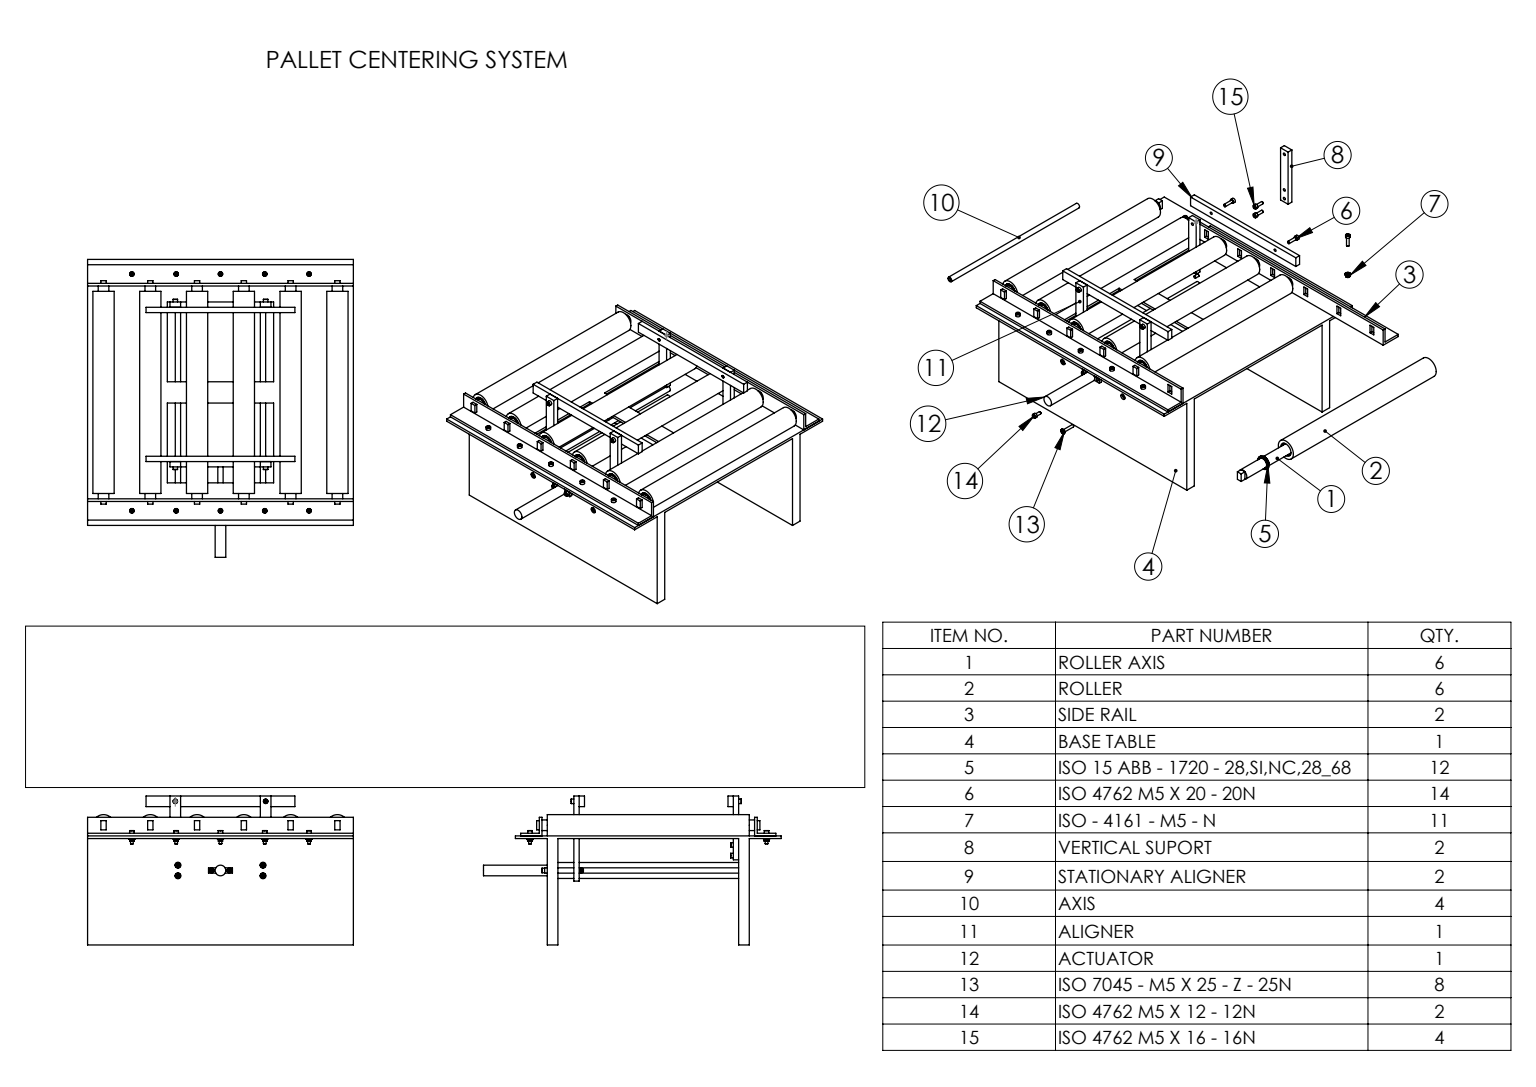
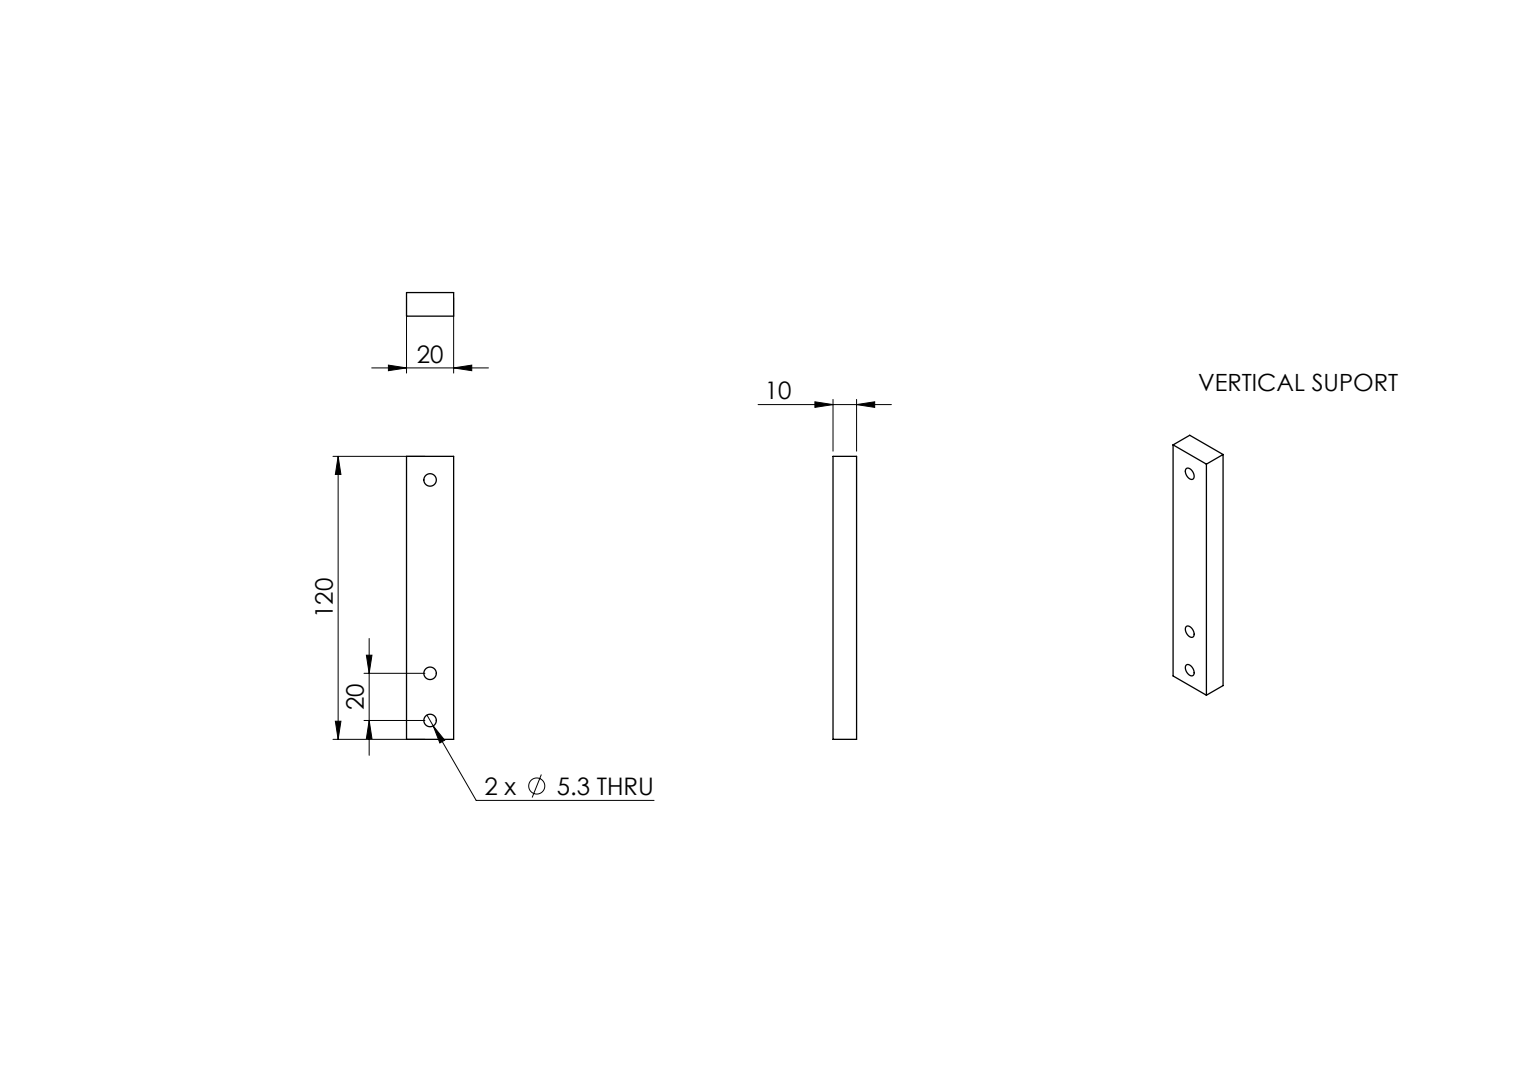
ISO-10303-21;
HEADER;
FILE_DESCRIPTION (('STEP AP214'),
    '1' );
FILE_NAME ('MAS-197',
    '2026-10-24T13:33:06',
    ( '' ),
    ( '' ),
    'SwSTEP 2.0',
    'SolidWorks 2026',
    '' );
FILE_SCHEMA (( 'AUTOMOTIVE_DESIGN' ));
ENDSEC;

DATA;
#1 = CARTESIAN_POINT ( 'NONE',  ( 53.33333333333330017, -25.00000000000000000, 222.5000000000000853 ) ) ;
#2 = AXIS2_PLACEMENT_3D ( 'NONE', #1029, #14245, #1184 ) ;
#3 = ORIENTED_EDGE ( 'NONE', *, *, #4024, .T. ) ;
#4 = CARTESIAN_POINT ( 'NONE',  ( 302.6499999999999204, -75.00000000000008527, 169.9999999999999716 ) ) ;
#5 = CARTESIAN_POINT ( 'NONE',  ( 136.6666666666666288, -20.00000000000000000, -219.8500000000001080 ) ) ;
#6 = DIRECTION ( 'NONE',  ( 0.000000000000000000, 0.000000000000000000, -1.000000000000000000 ) ) ;
#7 = EDGE_LOOP ( 'NONE', ( #4823, #10214, #8474, #13193, #10057 ) ) ;
#8 = COLOUR_RGB ( '',0.8941176470588234615, 0.8941176470588234615, 0.8941176470588234615 ) ;
#9 = EDGE_CURVE ( 'NONE', #9071, #5710, #2897, .T. ) ;
#10 = DIRECTION ( 'NONE',  ( 0.000000000000000000, 0.000000000000000000, -1.000000000000000000 ) ) ;
#11 = EDGE_CURVE ( 'NONE', #2602, #678, #10776, .T. ) ;
#12 = LINE ( 'NONE', #10262, #8342 ) ;
#13 = LINE ( 'NONE', #14246, #12970 ) ;
#14 = AXIS2_PLACEMENT_3D ( 'NONE', #7611, #4365, #10700 ) ;
#15 = DIRECTION ( 'NONE',  ( -0.000000000000000000, -0.000000000000000000, -1.000000000000000000 ) ) ;
#16 = EDGE_CURVE ( 'NONE', #12113, #10379, #13864, .T. ) ;
#17 = ORIENTED_EDGE ( 'NONE', *, *, #13765, .F. ) ;
#18 = MECHANICAL_DESIGN_GEOMETRIC_PRESENTATION_REPRESENTATION (  '', ( #6765 ), #7674 ) ;
#19 = DIRECTION ( 'NONE',  ( 1.000000000000000000, 0.000000000000000000, 0.000000000000000000 ) ) ;
#20 = DIRECTION ( 'NONE',  ( 1.000000000000000000, 0.000000000000000000, 0.000000000000000000 ) ) ;
#21 = VECTOR ( 'NONE', #6060, 1000.000000000000000 ) ;
#22 = CARTESIAN_POINT ( 'NONE',  ( 137.4999999999999432, -36.99999999999997868, -180.0000000000000000 ) ) ;
#23 = ORIENTED_EDGE ( 'NONE', *, *, #5278, .F. ) ;
#24 = CYLINDRICAL_SURFACE ( 'NONE', #7328, 2.649999999999985700 ) ;
#25 = AXIS2_PLACEMENT_3D ( 'NONE', #8308, #3030, #675 ) ;
#26 = COLOUR_RGB ( '',0.8941176470588234615, 0.8941176470588234615, 0.8941176470588234615 ) ;
#27 = DIRECTION ( 'NONE',  ( -0.000000000000000000, 0.000000000000000000, -1.000000000000000000 ) ) ;
#28 = VECTOR ( 'NONE', #11250, 999.9999999999997726 ) ;
#29 = CARTESIAN_POINT ( 'NONE',  ( 302.6499999999999204, -75.00000000000008527, 186.2999999999999829 ) ) ;
#30 = DIRECTION ( 'NONE',  ( 1.000000000000000000, 6.123233995736766036E-17, -6.123233995736764803E-17 ) ) ;
#31 = AXIS2_PLACEMENT_3D ( 'NONE', #13162, #68, #13234 ) ;
#32 = VERTEX_POINT ( 'NONE', #10617 ) ;
#33 = DIRECTION ( 'NONE',  ( -1.000000000000000000, -0.000000000000000000, -0.000000000000000000 ) ) ;
#34 = EDGE_CURVE ( 'NONE', #3584, #3648, #12190, .T. ) ;
#35 =( GEOMETRIC_REPRESENTATION_CONTEXT ( 3 ) GLOBAL_UNCERTAINTY_ASSIGNED_CONTEXT ( ( #12045 ) ) GLOBAL_UNIT_ASSIGNED_CONTEXT ( ( #1891, #1958, #13996 ) ) REPRESENTATION_CONTEXT ( 'NONE', 'WORKASPACE' ) );
#36 = ORIENTED_EDGE ( 'NONE', *, *, #2375, .F. ) ;
#37 = ADVANCED_FACE ( 'NONE', ( #11695 ), #12926, .T. ) ;
#38 = CARTESIAN_POINT ( 'NONE',  ( 4.175648173966055587, -2.207990556236547608, -3.469390959564065291 ) ) ;
#39 = ORIENTED_EDGE ( 'NONE', *, *, #7804, .T. ) ;
#40 = ORIENTED_EDGE ( 'NONE', *, *, #13656, .T. ) ;
#41 = CARTESIAN_POINT ( 'NONE',  ( 2.000000000000001332, 13.29999999999999893, 0.000000000000000000 ) ) ;
#42 = FACE_OUTER_BOUND ( 'NONE', #11021, .T. ) ;
#43 = CIRCLE ( 'NONE', #4245, 0.2000000000000000944 ) ;
#44 = DIRECTION ( 'NONE',  ( -0.000000000000000000, -0.000000000000000000, 1.000000000000000000 ) ) ;
#45 = CARTESIAN_POINT ( 'NONE',  ( 386.6666666666666288, -20.00000000000000000, 225.1500000000000625 ) ) ;
#46 = FACE_OUTER_BOUND ( 'NONE', #11584, .T. ) ;
#47 = CARTESIAN_POINT ( 'NONE',  ( -30.00000000000002842, -25.00000000000000000, 250.0000000000000000 ) ) ;
#48 = PLANE ( 'NONE',  #10641 ) ;
#49 = DIRECTION ( 'NONE',  ( 1.000000000000000000, 0.000000000000000000, 0.000000000000000000 ) ) ;
#50 = VERTEX_POINT ( 'NONE', #7335 ) ;
#51 = ORIENTED_EDGE ( 'NONE', *, *, #14217, .F. ) ;
#52 = FACE_OUTER_BOUND ( 'NONE', #5422, .T. ) ;
#53 = ORIENTED_EDGE ( 'NONE', *, *, #841, .T. ) ;
#54 = CARTESIAN_POINT ( 'NONE',  ( -299.9999999999999432, -75.00000000000008527, 329.9999999999999432 ) ) ;
#55 = ORIENTED_EDGE ( 'NONE', *, *, #9775, .T. ) ;
#56 = DIRECTION ( 'NONE',  ( 1.000000000000000000, 0.000000000000000000, 0.000000000000000000 ) ) ;
#57 = ORIENTED_EDGE ( 'NONE', *, *, #5179, .T. ) ;
#58 = CARTESIAN_POINT ( 'NONE',  ( -297.4999999999999432, -75.00000000000008527, 10.00000000000000178 ) ) ;
#59 = PRODUCT ( 'MAS-197', 'MAS-197', '', ( #13427 ) ) ;
#60 = CARTESIAN_POINT ( 'NONE',  ( 4.000000000000000000, 2.309401076758497151, -3.433295621305379353 ) ) ;
#61 = DIRECTION ( 'NONE',  ( -1.000000000000000000, -0.000000000000000000, -0.000000000000000000 ) ) ;
#62 = EDGE_CURVE ( 'NONE', #11600, #2281, #14003, .T. ) ;
#63 = CARTESIAN_POINT ( 'NONE',  ( 2.500000000000000000, 0.000000000000000000, 0.000000000000000000 ) ) ;
#64 = EDGE_CURVE ( 'NONE', #764, #13509, #648, .T. ) ;
#65 = CARTESIAN_POINT ( 'NONE',  ( -30.00000000000002842, -20.00000000000000000, 250.0000000000000000 ) ) ;
#66 = ORIENTED_EDGE ( 'NONE', *, *, #8156, .T. ) ;
#67 = VERTEX_POINT ( 'NONE', #13720 ) ;
#68 = DIRECTION ( 'NONE',  ( 1.000000000000000000, 0.000000000000000000, 0.000000000000000000 ) ) ;
#69 = ORIENTED_EDGE ( 'NONE', *, *, #9344, .T. ) ;
#70 = DIRECTION ( 'NONE',  ( 0.000000000000000000, 1.000000000000000000, 0.000000000000000000 ) ) ;
#71 = CYLINDRICAL_SURFACE ( 'NONE', #9896, 2.500000000000000444 ) ;
#72 =( NAMED_UNIT ( * ) SI_UNIT ( $, .STERADIAN. ) SOLID_ANGLE_UNIT ( ) );
#73 =( REPRESENTATION_RELATIONSHIP ('NONE','NONE', #11251, #2275 ) REPRESENTATION_RELATIONSHIP_WITH_TRANSFORMATION ( #10001 )SHAPE_REPRESENTATION_RELATIONSHIP( ) );
#74 = EDGE_CURVE ( 'NONE', #2665, #8392, #9526, .T. ) ;
#75 = PRODUCT_DEFINITION ( 'UNKNOWN', '', #10251, #12968 ) ;
#76 = LINE ( 'NONE', #7062, #6983 ) ;
#77 = FACE_OUTER_BOUND ( 'NONE', #3479, .T. ) ;
#78 = PLANE ( 'NONE',  #3254 ) ;
#79 = DIRECTION ( 'NONE',  ( 1.000000000000000000, 0.000000000000000000, 0.000000000000000000 ) ) ;
#80 = EDGE_LOOP ( 'NONE', ( #13793, #10829, #6578 ) ) ;
#81 = ADVANCED_FACE ( 'NONE', ( #7413, #11845, #1899, #419, #4888, #9306, #3544 ), #4372, .T. ) ;
#82 = EDGE_CURVE ( 'NONE', #232, #4077, #12381, .T. ) ;
#83 = AXIS2_PLACEMENT_3D ( 'NONE', #9067, #7962, #321 ) ;
#84 = AXIS2_PLACEMENT_3D ( 'NONE', #4836, #3666, #8077 ) ;
#85 = EDGE_CURVE ( 'NONE', #6756, #11518, #12060, .T. ) ;
#86 = ADVANCED_FACE ( 'NONE', ( #14292 ), #14148, .F. ) ;
#87 = CARTESIAN_POINT ( 'NONE',  ( 134.9999999999999432, -36.99999999999997868, 0.000000000000000000 ) ) ;
#88 = LINE ( 'NONE', #2296, #2370 ) ;
#89 = PLANE ( 'NONE',  #11765 ) ;
#90 = ORIENTED_EDGE ( 'NONE', *, *, #8678, .T. ) ;
#91 = ADVANCED_FACE ( 'NONE', ( #1003 ), #2259, .T. ) ;
#92 = CARTESIAN_POINT ( 'NONE',  ( -144.9999999999999432, -105.0000000000000853, 40.00000000000000000 ) ) ;
#93 = CARTESIAN_POINT ( 'NONE',  ( 2.500000000000000000, 2.357898499370433054, -1.951563910473907981E-15 ) ) ;
#94 = DIRECTION ( 'NONE',  ( 0.000000000000000000, 0.000000000000000000, 1.000000000000000000 ) ) ;
#95 = CIRCLE ( 'NONE', #11951, 2.700000000000000178 ) ;
#96 = ORIENTED_EDGE ( 'NONE', *, *, #5946, .F. ) ;
#97 = LINE ( 'NONE', #13393, #5781 ) ;
#98 = ORIENTED_EDGE ( 'NONE', *, *, #4977, .T. ) ;
#99 = CARTESIAN_POINT ( 'NONE',  ( 4.999999999999997335, 0.000000000000000000, 4.250000000000000000 ) ) ;
#100 = VECTOR ( 'NONE', #4876, 1000.000000000000000 ) ;
#101 = ORIENTED_EDGE ( 'NONE', *, *, #7387, .T. ) ;
#102 = ORIENTED_EDGE ( 'NONE', *, *, #13999, .T. ) ;
#103 = DIRECTION ( 'NONE',  ( -1.000000000000000000, 0.000000000000000000, 0.000000000000000000 ) ) ;
#104 = DIRECTION ( 'NONE',  ( 0.000000000000000000, 0.000000000000000000, 1.000000000000000000 ) ) ;
#105 = CARTESIAN_POINT ( 'NONE',  ( 5.000000000000000888, 0.000000000000000000, 0.000000000000000000 ) ) ;
#106 = DIRECTION ( 'NONE',  ( 0.4461977533473793778, 0.8949343913984707521, -1.884057886186824495E-16 ) ) ;
#107 = LINE ( 'NONE', #12182, #1892 ) ;
#108 = LINE ( 'NONE', #6679, #5937 ) ;
#109 = SURFACE_STYLE_FILL_AREA ( #5656 ) ;
#110 = EDGE_CURVE ( 'NONE', #13194, #10462, #10760, .T. ) ;
#111 = CARTESIAN_POINT ( 'NONE',  ( 132.4999999999999432, -36.99999999999997868, -169.9999999999999716 ) ) ;
#112 = ITEM_DEFINED_TRANSFORMATION ( 'NONE', 'NONE', #8858,  #14039 ) ;
#113 = CIRCLE ( 'NONE', #1517, 5.500000000000005329 ) ;
#114 = ORIENTED_EDGE ( 'NONE', *, *, #1574, .F. ) ;
#115 = ORIENTED_EDGE ( 'NONE', *, *, #82, .F. ) ;
#116 = AXIS2_PLACEMENT_3D ( 'NONE', #1990, #12809, #3959 ) ;
#117 = CARTESIAN_POINT ( 'NONE',  ( 0.06760930072668894231, 0.9010842325122832008, -0.5150000000000000133 ) ) ;
#118 = ORIENTED_EDGE ( 'NONE', *, *, #14031, .F. ) ;
#119 = CARTESIAN_POINT ( 'NONE',  ( 134.5000000000000000, -95.00000000000008527, 190.0000000000000000 ) ) ;
#120 = AXIS2_PLACEMENT_3D ( 'NONE', #1147, #9264, #49 ) ;
#121 = ORIENTED_EDGE ( 'NONE', *, *, #4725, .F. ) ;
#122 = LINE ( 'NONE', #2191, #4564 ) ;
#123 = ORIENTED_EDGE ( 'NONE', *, *, #13765, .T. ) ;
#124 = CARTESIAN_POINT ( 'NONE',  ( 142.6500000000000057, -95.00000000000008527, 190.0000000000000000 ) ) ;
#125 = AXIS2_PLACEMENT_3D ( 'NONE', #612, #5076, #9487 ) ;
#126 = CARTESIAN_POINT ( 'NONE',  ( 4.000000000000000888, 1.539600717838996990, -3.300726591567079815 ) ) ;
#127 = DIRECTION ( 'NONE',  ( 0.000000000000000000, 0.000000000000000000, 1.000000000000000000 ) ) ;
#128 = AXIS2_PLACEMENT_3D ( 'NONE', #6258, #5252, #1681 ) ;
#129 = CARTESIAN_POINT ( 'NONE',  ( 357.0000000000000000, 8.660254037844390851, 205.0000000000000284 ) ) ;
#130 = FILL_AREA_STYLE ('',( #3509 ) ) ;
#131 = DIRECTION ( 'NONE',  ( 0.4461977533474923430, -0.8949343913984144638, 0.000000000000000000 ) ) ;
#132 = DIRECTION ( 'NONE',  ( 1.000000000000000000, 0.000000000000000000, 0.000000000000000000 ) ) ;
#133 = DIRECTION ( 'NONE',  ( 1.000000000000000000, 0.000000000000000000, 0.000000000000000000 ) ) ;
#134 = VECTOR ( 'NONE', #9384, 1000.000000000000000 ) ;
#135 =( REPRESENTATION_RELATIONSHIP ('NONE','NONE', #11251, #5332 ) REPRESENTATION_RELATIONSHIP_WITH_TRANSFORMATION ( #4005 )SHAPE_REPRESENTATION_RELATIONSHIP( ) );
#136 = EDGE_LOOP ( 'NONE', ( #496, #11440, #13448, #1824 ) ) ;
#137 = ORIENTED_EDGE ( 'NONE', *, *, #8244, .F. ) ;
#138 = VECTOR ( 'NONE', #5329, 1000.000000000000000 ) ;
#139 = B_SPLINE_CURVE_WITH_KNOTS ( 'NONE', 3,
 ( #12728, #3886, #6926, #516, #12587, #8082 ),
 .UNSPECIFIED., .F., .F.,
 ( 4, 2, 4 ),
 ( 0.002365888236227967761, 0.003551327329835077609, 0.004736766423442186590 ),
 .UNSPECIFIED. ) ;
#140 = VERTEX_POINT ( 'NONE', #5318 ) ;
#141 = ADVANCED_FACE ( 'NONE', ( #13281 ), #9741, .F. ) ;
#143 = CARTESIAN_POINT ( 'NONE',  ( 93.00000000000000000, -8.660254037844389075, 199.9990000000000236 ) ) ;
#142 = AXIS2_PLACEMENT_3D ( 'NONE', #8631, #1337, #6858 ) ;
#144 = VECTOR ( 'NONE', #12485, 1000.000000000000000 ) ;
#145 = VERTEX_POINT ( 'NONE', #3075 ) ;
#146 = CARTESIAN_POINT ( 'NONE',  ( 0.000000000000000000, -2.349999999999999201, 0.5149999999999992362 ) ) ;
#147 = DIRECTION ( 'NONE',  ( 0.000000000000000000, 0.000000000000000000, 1.000000000000000000 ) ) ;
#148 = CIRCLE ( 'NONE', #8278, 4.000000000000000000 ) ;
#149 = AXIS2_PLACEMENT_3D ( 'NONE', #12993, #2990, #1889 ) ;
#150 = LINE ( 'NONE', #1253, #5148 ) ;
#151 = FACE_OUTER_BOUND ( 'NONE', #9117, .T. ) ;
#152 = AXIS2_PLACEMENT_3D ( 'NONE', #10051, #218, #9907 ) ;
#153 = PLANE ( 'NONE',  #6564 ) ;
#154 = DIRECTION ( 'NONE',  ( 1.000000000000000000, 0.000000000000000000, 0.000000000000000000 ) ) ;
#155 = EDGE_LOOP ( 'NONE', ( #7067, #11901, #14288, #9379, #2172, #12925 ) ) ;
#156 = ADVANCED_FACE ( 'NONE', ( #2113 ), #8789, .F. ) ;
#157 = DIRECTION ( 'NONE',  ( -0.000000000000000000, -0.000000000000000000, 1.000000000000000000 ) ) ;
#158 = CYLINDRICAL_SURFACE ( 'NONE', #4474, 2.649999999999985700 ) ;
#159=STYLED_ITEM('',(#14424),#13163);
#160 = CARTESIAN_POINT ( 'NONE',  ( 2.500000000000000000, -1.178949249685218303, -2.041999999999998039 ) ) ;
#161 = VERTEX_POINT ( 'NONE', #11045 ) ;
#162 = DIRECTION ( 'NONE',  ( -0.000000000000000000, -0.000000000000000000, 1.000000000000000000 ) ) ;
#163 = ADVANCED_FACE ( 'NONE', ( #5247 ), #3288, .T. ) ;
#164 = EDGE_CURVE ( 'NONE', #13531, #14219, #11463, .T. ) ;
#165 = CARTESIAN_POINT ( 'NONE',  ( 5.000000000000000888, 4.250000000000000000, 0.000000000000000000 ) ) ;
#166 = DIRECTION ( 'NONE',  ( 1.000000000000000000, 0.000000000000000000, 0.000000000000000000 ) ) ;
#167 = EDGE_CURVE ( 'NONE', #11965, #7113, #13067, .T. ) ;
#168 = VECTOR ( 'NONE', #12487, 1000.000000000000000 ) ;
#169 = ITEM_DEFINED_TRANSFORMATION ( 'NONE', 'NONE', #949,  #14039 ) ;
#170 = ORIENTED_EDGE ( 'NONE', *, *, #8134, .F. ) ;
#171 = CIRCLE ( 'NONE', #3238, 20.00000000000000000 ) ;
#172 = CARTESIAN_POINT ( 'NONE',  ( 21.00000000000000355, 0.000000000000000000, 0.000000000000000000 ) ) ;
#173 = PRODUCT ( 'base table', 'base table', '', ( #338 ) ) ;
#174 = B_SPLINE_CURVE_WITH_KNOTS ( 'NONE', 3,
 ( #13860, #2775, #7121, #12779, #11548 ),
 .UNSPECIFIED., .F., .F.,
 ( 4, 1, 4 ),
 ( 0.000000000000000000, 0.002309401076758506657, 0.004618802153517013315 ),
 .UNSPECIFIED. ) ;
#175 = ORIENTED_EDGE ( 'NONE', *, *, #6775, .T. ) ;
#176 = DIRECTION ( 'NONE',  ( -0.000000000000000000, 1.000000000000000000, 0.000000000000000000 ) ) ;
#177 = CIRCLE ( 'NONE', #2061, 2.500000000000002220 ) ;
#178 = ORIENTED_EDGE ( 'NONE', *, *, #7566, .F. ) ;
#179 = ORIENTED_EDGE ( 'NONE', *, *, #5778, .F. ) ;
#180 = CARTESIAN_POINT ( 'NONE',  ( 299.9999999999999432, -95.00000000000008527, 190.0000000000000000 ) ) ;
#181 = CARTESIAN_POINT ( 'NONE',  ( 302.6499999999999204, -95.00000000000008527, -186.2999999999999829 ) ) ;
#182 = CARTESIAN_POINT ( 'NONE',  ( 2.500000000000000000, -1.768423874527823791, -1.020999999999998353 ) ) ;
#183 = VECTOR ( 'NONE', #12816, 1000.000000000000000 ) ;
#184 = FACE_OUTER_BOUND ( 'NONE', #8422, .T. ) ;
#185 = DIRECTION ( 'NONE',  ( 1.000000000000000000, 0.000000000000000000, 0.000000000000000000 ) ) ;
#186 = DIRECTION ( 'NONE',  ( 1.000000000000000000, 0.000000000000000000, 0.000000000000000000 ) ) ;
#187 =( LENGTH_UNIT ( ) NAMED_UNIT ( * ) SI_UNIT ( .MILLI., .METRE. ) );
#188 = EDGE_CURVE ( 'NONE', #1051, #13344, #1074, .T. ) ;
#189 = CARTESIAN_POINT ( 'NONE',  ( 4.207491450040567571, -2.029819825146485179, -3.671670828759567407 ) ) ;
#190 = EDGE_LOOP ( 'NONE', ( #1618, #1963 ) ) ;
#191 = VERTEX_POINT ( 'NONE', #7546 ) ;
#192 = CARTESIAN_POINT ( 'NONE',  ( 303.3333333333333144, -20.00000000000000000, -219.8500000000001080 ) ) ;
#193 = ORIENTED_EDGE ( 'NONE', *, *, #7276, .F. ) ;
#194 = DIRECTION ( 'NONE',  ( 1.000000000000000000, 0.000000000000000000, 0.000000000000000000 ) ) ;
#195 = CIRCLE ( 'NONE', #13619, 2.500000000000002220 ) ;
#196 = EDGE_LOOP ( 'NONE', ( #178, #7479, #11699, #10408 ) ) ;
#197 = DIRECTION ( 'NONE',  ( -0.000000000000000000, -0.000000000000000000, -1.000000000000000000 ) ) ;
#198 = ORIENTED_EDGE ( 'NONE', *, *, #12237, .T. ) ;
#199 = AXIS2_PLACEMENT_3D ( 'NONE', #13030, #8676, #7512 ) ;
#200 = CARTESIAN_POINT ( 'NONE',  ( -294.9999999999999432, -75.00000000000008527, 339.9999999999999432 ) ) ;
#201 = CARTESIAN_POINT ( 'NONE',  ( 294.4999999999999432, -75.00000000000008527, -190.0000000000000000 ) ) ;
#202 = DIRECTION ( 'NONE',  ( -0.000000000000000000, 0.000000000000000000, -1.000000000000000000 ) ) ;
#203 = DIRECTION ( 'NONE',  ( 0.000000000000000000, 0.000000000000000000, 1.000000000000000000 ) ) ;
#204 = PRESENTATION_STYLE_ASSIGNMENT (( #4594 ) ) ;
#205 = CYLINDRICAL_SURFACE ( 'NONE', #8810, 11.05000000000000071 ) ;
#206 = SHAPE_DEFINITION_REPRESENTATION ( #7042, #11251 ) ;
#207 = DIRECTION ( 'NONE',  ( 0.000000000000000000, -0.000000000000000000, 1.000000000000000000 ) ) ;
#208 = SHAPE_REPRESENTATION ( 'angular contact ball bearing_68_iso_ISO 15 ABB - 1720 - 28,SI,NC,28_68', ( #14039 ), #11646 ) ;
#209 = ORIENTED_EDGE ( 'NONE', *, *, #9578, .T. ) ;
#210 = ORIENTED_EDGE ( 'NONE', *, *, #2503, .T. ) ;
#211 = ORIENTED_EDGE ( 'NONE', *, *, #1146, .F. ) ;
#212 = VECTOR ( 'NONE', #10286, 1000.000000000000114 ) ;
#213 = CARTESIAN_POINT ( 'NONE',  ( 3.383466608491643077E-15, 4.736522675502341073, -3.681124513963742739 ) ) ;
#214 = EDGE_CURVE ( 'NONE', #1600, #9602, #14242, .T. ) ;
#215 = ORIENTED_EDGE ( 'NONE', *, *, #12757, .F. ) ;
#216 = CYLINDRICAL_SURFACE ( 'NONE', #14049, 4.250000000000000000 ) ;
#217 = PLANE ( 'NONE',  #14054 ) ;
#218 = DIRECTION ( 'NONE',  ( -1.000000000000000000, -0.000000000000000000, -0.000000000000000000 ) ) ;
#219 = CIRCLE ( 'NONE', #5381, 5.000000000000004441 ) ;
#220 = AXIS2_PLACEMENT_3D ( 'NONE', #2707, #9091, #281 ) ;
#221 = CARTESIAN_POINT ( 'NONE',  ( -25.39999999999996305, 0.000000000000000000, 0.000000000000000000 ) ) ;
#222 = VECTOR ( 'NONE', #1616, 1000.000000000000000 ) ;
#223 = LINE ( 'NONE', #12223, #5365 ) ;
#224 = CARTESIAN_POINT ( 'NONE',  ( -219.9999999999999147, -85.00000000000009948, 30.00000000000000000 ) ) ;
#225 = CARTESIAN_POINT ( 'NONE',  ( 8.000000000000000000, -4.837354856632045452E-15, -0.5150000000000000133 ) ) ;
#226 = EDGE_LOOP ( 'NONE', ( #6646, #8713, #11419, #2781 ) ) ;
#227 = FILL_AREA_STYLE ('',( #2582 ) ) ;
#228 = AXIS2_PLACEMENT_3D ( 'NONE', #3013, #14095, #2869 ) ;
#229 = DIRECTION ( 'NONE',  ( -0.000000000000000000, -0.000000000000000000, -1.000000000000000000 ) ) ;
#230 = LINE ( 'NONE', #296, #13478 ) ;
#231 = LINE ( 'NONE', #7733, #9690 ) ;
#232 = VERTEX_POINT ( 'NONE', #2038 ) ;
#233 = FACE_OUTER_BOUND ( 'NONE', #9286, .T. ) ;
#234 = EDGE_CURVE ( 'NONE', #10453, #9107, #4526, .T. ) ;
#235 = AXIS2_PLACEMENT_3D ( 'NONE', #10662, #12975, #4053 ) ;
#236 = DIRECTION ( 'NONE',  ( 1.000000000000000000, 0.000000000000000000, 0.000000000000000000 ) ) ;
#237 = DIRECTION ( 'NONE',  ( 0.000000000000000000, 0.000000000000000000, 1.000000000000000000 ) ) ;
#238 = EDGE_CURVE ( 'NONE', #5881, #9436, #12617, .T. ) ;
#239 = ORIENTED_EDGE ( 'NONE', *, *, #12866, .T. ) ;
#240 = DIRECTION ( 'NONE',  ( 0.000000000000000000, 1.000000000000000000, -1.224646799147353207E-16 ) ) ;
#241 = AXIS2_PLACEMENT_3D ( 'NONE', #10628, #13202, #658 ) ;
#242 = ORIENTED_EDGE ( 'NONE', *, *, #12141, .F. ) ;
#243 = CARTESIAN_POINT ( 'NONE',  ( 4.141042297810615835, -2.227970268150433863, -3.687027686973623819 ) ) ;
#244 = ADVANCED_FACE ( 'NONE', ( #3220 ), #6544, .F. ) ;
#245 = AXIS2_PLACEMENT_3D ( 'NONE', #11200, #8675, #5417 ) ;
#246 = VERTEX_POINT ( 'NONE', #11184 ) ;
#247 = VERTEX_POINT ( 'NONE', #2541 ) ;
#248 = DIRECTION ( 'NONE',  ( -0.000000000000000000, -0.000000000000000000, -1.000000000000000000 ) ) ;
#249 = CARTESIAN_POINT ( 'NONE',  ( 2.756197834950227410, 3.027510591568626896, -3.223146290109805356 ) ) ;
#250 = DIRECTION ( 'NONE',  ( 1.000000000000000000, 0.000000000000000000, 0.000000000000000000 ) ) ;
#251 = EDGE_CURVE ( 'NONE', #12108, #865, #13488, .T. ) ;
#252 = CARTESIAN_POINT ( 'NONE',  ( 307.5000000000000000, -56.99999999999997158, -180.0000000000000000 ) ) ;
#253 = CARTESIAN_POINT ( 'NONE',  ( -2.000000000000002665, -3.464101615137770374, -3.142992957459237680 ) ) ;
#254 = DIRECTION ( 'NONE',  ( -1.000000000000000000, 0.000000000000000000, 0.000000000000000000 ) ) ;
#255 = CARTESIAN_POINT ( 'NONE',  ( 119.9999999999999147, -20.00000000000000000, 19.99999999999998934 ) ) ;
#256 =( GEOMETRIC_REPRESENTATION_CONTEXT ( 3 ) GLOBAL_UNCERTAINTY_ASSIGNED_CONTEXT ( ( #4951 ) ) GLOBAL_UNIT_ASSIGNED_CONTEXT ( ( #9085, #1379, #10099 ) ) REPRESENTATION_CONTEXT ( 'NONE', 'WORKASPACE' ) );
#257 = ORIENTED_EDGE ( 'NONE', *, *, #9709, .T. ) ;
#258 = VERTEX_POINT ( 'NONE', #13414 ) ;
#259 = DIRECTION ( 'NONE',  ( 0.000000000000000000, 0.000000000000000000, 1.000000000000000000 ) ) ;
#260 =( REPRESENTATION_RELATIONSHIP ('NONE','NONE', #11251, #5332 ) REPRESENTATION_RELATIONSHIP_WITH_TRANSFORMATION ( #8928 )SHAPE_REPRESENTATION_RELATIONSHIP( ) );
#261 = ORIENTED_EDGE ( 'NONE', *, *, #3754, .T. ) ;
#262 = DIRECTION ( 'NONE',  ( -1.000000000000000000, 0.000000000000000000, 0.000000000000000000 ) ) ;
#263 = EDGE_CURVE ( 'NONE', #5128, #8193, #4654, .T. ) ;
#264 = CIRCLE ( 'NONE', #6784, 2.500000000000000444 ) ;
#265 = ORIENTED_EDGE ( 'NONE', *, *, #11090, .F. ) ;
#266 = EDGE_CURVE ( 'NONE', #11339, #3317, #13546, .T. ) ;
#267 = CARTESIAN_POINT ( 'NONE',  ( 319.9999999999999432, -225.0010000000000048, 19.99999999999998934 ) ) ;
#268 = ORIENTED_EDGE ( 'NONE', *, *, #5003, .F. ) ;
#269 = LINE ( 'NONE', #13422, #9164 ) ;
#270 = AXIS2_PLACEMENT_3D ( 'NONE', #3591, #10188, #1328 ) ;
#271 = FACE_OUTER_BOUND ( 'NONE', #11503, .T. ) ;
#272 = ORIENTED_EDGE ( 'NONE', *, *, #4554, .T. ) ;
#273 = ADVANCED_FACE ( 'NONE', ( #9135 ), #3628, .F. ) ;
#274 = CARTESIAN_POINT ( 'NONE',  ( 242.5000000000000000, -90.00000000000007105, 55.00000000000001421 ) ) ;
#275 = SURFACE_STYLE_FILL_AREA ( #9302 ) ;
#276 = CARTESIAN_POINT ( 'NONE',  ( 134.9999999999999716, 45.00000000000001421, -174.9999999999999716 ) ) ;
#277 = LINE ( 'NONE', #1310, #12003 ) ;
#278 = VERTEX_POINT ( 'NONE', #12335 ) ;
#279 = ORIENTED_EDGE ( 'NONE', *, *, #5164, .T. ) ;
#280 = EDGE_LOOP ( 'NONE', ( #548, #583, #6220, #3150 ) ) ;
#281 = DIRECTION ( 'NONE',  ( 0.000000000000000000, 0.000000000000000000, -1.000000000000000000 ) ) ;
#282 = ORIENTED_EDGE ( 'NONE', *, *, #2329, .T. ) ;
#283 = CARTESIAN_POINT ( 'NONE',  ( 2.500000000000000000, -1.178949249685214307, 2.042000000000001592 ) ) ;
#284 = ORIENTED_EDGE ( 'NONE', *, *, #11720, .T. ) ;
#285 = CARTESIAN_POINT ( 'NONE',  ( 259.0000000000000000, 8.660254037844390851, 205.0000000000000284 ) ) ;
#286 = CARTESIAN_POINT ( 'NONE',  ( 2.740000000000000213, 0.5149999999999976819, 0.6774776749089244099 ) ) ;
#287 = DIRECTION ( 'NONE',  ( -0.000000000000000000, -1.000000000000000000, -0.000000000000000000 ) ) ;
#288 = DIRECTION ( 'NONE',  ( 0.000000000000000000, 0.000000000000000000, 1.000000000000000000 ) ) ;
#289 = SURFACE_STYLE_FILL_AREA ( #9245 ) ;
#290 = DIRECTION ( 'NONE',  ( -0.000000000000000000, 1.000000000000000000, -0.000000000000000000 ) ) ;
#291 = PRODUCT_DEFINITION_SHAPE ( 'NONE', 'NONE',  #3819 ) ;
#292 = DIRECTION ( 'NONE',  ( 0.000000000000000000, 0.000000000000000000, -1.000000000000000000 ) ) ;
#293 = EDGE_CURVE ( 'NONE', #12041, #2215, #4727, .T. ) ;
#294 = ORIENTED_EDGE ( 'NONE', *, *, #6857, .T. ) ;
#295 = CARTESIAN_POINT ( 'NONE',  ( 302.6499999999999204, -75.00000000000008527, 186.2999999999999829 ) ) ;
#296 = CARTESIAN_POINT ( 'NONE',  ( 2.500000000000000000, 1.178949249685218525, 2.041999999999999371 ) ) ;
#297 = DIRECTION ( 'NONE',  ( -0.000000000000000000, 0.8660254037844390407, 0.4999999999999993339 ) ) ;
#298 = VERTEX_POINT ( 'NONE', #6685 ) ;
#299 = DIRECTION ( 'NONE',  ( -0.000000000000000000, -0.000000000000000000, 1.000000000000000000 ) ) ;
#300 = FACE_OUTER_BOUND ( 'NONE', #11789, .T. ) ;
#301 = CARTESIAN_POINT ( 'NONE',  ( 53.33333333333330017, -10.00000000000000000, -222.5000000000000853 ) ) ;
#302 = EDGE_CURVE ( 'NONE', #5376, #611, #2399, .T. ) ;
#303 = FACE_OUTER_BOUND ( 'NONE', #3913, .T. ) ;
#304 = ORIENTED_EDGE ( 'NONE', *, *, #14182, .F. ) ;
#305 = DIRECTION ( 'NONE',  ( -1.000000000000000000, -0.000000000000000000, -0.000000000000000000 ) ) ;
#306 = EDGE_LOOP ( 'NONE', ( #4499, #12572, #12024, #6931 ) ) ;
#307 = FACE_OUTER_BOUND ( 'NONE', #226, .T. ) ;
#308 = EDGE_CURVE ( 'NONE', #574, #7171, #11477, .T. ) ;
#309 = ORIENTED_EDGE ( 'NONE', *, *, #12893, .T. ) ;
#310 = ORIENTED_EDGE ( 'NONE', *, *, #2589, .F. ) ;
#311 = DIRECTION ( 'NONE',  ( -0.000000000000000000, 1.000000000000000000, 0.000000000000000000 ) ) ;
#312 = CARTESIAN_POINT ( 'NONE',  ( -304.9999999999999432, 45.00000000000001421, 30.00000000000000000 ) ) ;
#313 =( NAMED_UNIT ( * ) SI_UNIT ( $, .STERADIAN. ) SOLID_ANGLE_UNIT ( ) );
#314 = DIRECTION ( 'NONE',  ( -1.000000000000000000, -0.000000000000000000, -0.000000000000000000 ) ) ;
#315 = CARTESIAN_POINT ( 'NONE',  ( 304.9999999999999432, 45.00000000000001421, 0.000000000000000000 ) ) ;
#316 = CARTESIAN_POINT ( 'NONE',  ( 134.9999999999999432, -36.99999999999997868, 10.00000000000000000 ) ) ;
#317 = DIRECTION ( 'NONE',  ( 0.000000000000000000, 0.000000000000000000, 1.000000000000000000 ) ) ;
#318 = ITEM_DEFINED_TRANSFORMATION ( 'NONE', 'NONE', #3760,  #14039 ) ;
#319 = ORIENTED_EDGE ( 'NONE', *, *, #6736, .T. ) ;
#320 = EDGE_LOOP ( 'NONE', ( #13311, #10317 ) ) ;
#321 = DIRECTION ( 'NONE',  ( 0.000000000000000000, 0.000000000000000000, -1.000000000000000000 ) ) ;
#322 = AXIS2_PLACEMENT_3D ( 'NONE', #13350, #6899, #4588 ) ;
#323 = EDGE_LOOP ( 'NONE', ( #13718, #1656 ) ) ;
#324 = AXIS2_PLACEMENT_3D ( 'NONE', #905, #4134, #5226 ) ;
#325 = CARTESIAN_POINT ( 'NONE',  ( 142.6500000000000057, -75.00000000000008527, 186.2999999999999829 ) ) ;
#326 = EDGE_CURVE ( 'NONE', #2746, #3344, #2466, .T. ) ;
#327 = ADVANCED_FACE ( 'NONE', ( #11322 ), #1364, .F. ) ;
#328 = VERTEX_POINT ( 'NONE', #3699 ) ;
#329 = CARTESIAN_POINT ( 'NONE',  ( 2.500000000000000000, -1.768423874527823569, 1.021000000000002794 ) ) ;
#330 = ORIENTED_EDGE ( 'NONE', *, *, #1288, .T. ) ;
#331 = DIRECTION ( 'NONE',  ( 0.000000000000000000, 0.000000000000000000, 1.000000000000000000 ) ) ;
#332 = FACE_OUTER_BOUND ( 'NONE', #8846, .T. ) ;
#333 = ORIENTED_EDGE ( 'NONE', *, *, #6140, .F. ) ;
#334 = CARTESIAN_POINT ( 'NONE',  ( 0.3226060873438392207, -0.5150000000000068967, 2.189154565102729766 ) ) ;
#335 = DIRECTION ( 'NONE',  ( 0.000000000000000000, 1.000000000000000000, 0.000000000000000000 ) ) ;
#336 = CIRCLE ( 'NONE', #815, 5.500000000000005329 ) ;
#337 = PRESENTATION_STYLE_ASSIGNMENT (( #2631 ) ) ;
#338 = PRODUCT_CONTEXT ( 'NONE', #6572, 'mechanical' ) ;
#339 = EDGE_CURVE ( 'NONE', #9196, #8368, #11117, .T. ) ;
#340 = EDGE_CURVE ( 'NONE', #10091, #12864, #5804, .T. ) ;
#341 = CIRCLE ( 'NONE', #14262, 2.649999999999985700 ) ;
#342 = FACE_BOUND ( 'NONE', #10311, .T. ) ;
#343 = ORIENTED_EDGE ( 'NONE', *, *, #8371, .F. ) ;
#344 = EDGE_CURVE ( 'NONE', #3380, #915, #1258, .T. ) ;
#345 = ORIENTED_EDGE ( 'NONE', *, *, #12797, .F. ) ;
#346 = AXIS2_PLACEMENT_3D ( 'NONE', #5589, #5997, #454 ) ;
#347 = ORIENTED_EDGE ( 'NONE', *, *, #12633, .T. ) ;
#348 = LINE ( 'NONE', #12570, #6264 ) ;
#349 = AXIS2_PLACEMENT_3D ( 'NONE', #5295, #9713, #11738 ) ;
#350 = ORIENTED_EDGE ( 'NONE', *, *, #717, .F. ) ;
#351 = DIRECTION ( 'NONE',  ( -1.000000000000000000, -0.000000000000000000, -0.000000000000000000 ) ) ;
#352 = EDGE_LOOP ( 'NONE', ( #7551, #6628 ) ) ;
#353 = FACE_BOUND ( 'NONE', #877, .T. ) ;
#354 = AXIS2_PLACEMENT_3D ( 'NONE', #6912, #4747, #11272 ) ;
#355 = CARTESIAN_POINT ( 'NONE',  ( 79.99999999999971578, 55.00000000000000711, 0.000000000000000000 ) ) ;
#356 = AXIS2_PLACEMENT_3D ( 'NONE', #11452, #7091, #11525 ) ;
#357 = DIRECTION ( 'NONE',  ( 1.000000000000000000, 0.000000000000000000, 0.000000000000000000 ) ) ;
#358 = CARTESIAN_POINT ( 'NONE',  ( -30.00000000000002842, -225.0000000000000000, -169.9999999999999716 ) ) ;
#359 = VECTOR ( 'NONE', #3088, 1000.000000000000000 ) ;
#360 = DIRECTION ( 'NONE',  ( -1.000000000000000000, 0.000000000000000000, 0.000000000000000000 ) ) ;
#361 = CYLINDRICAL_SURFACE ( 'NONE', #6142, 12.77499999999999858 ) ;
#362 = ADVANCED_FACE ( 'NONE', ( #8113 ), #12549, .T. ) ;
#363 = CIRCLE ( 'NONE', #6654, 2.649999999999985700 ) ;
#364 = ORIENTED_EDGE ( 'NONE', *, *, #6973, .T. ) ;
#365 = VECTOR ( 'NONE', #9606, 1000.000000000000000 ) ;
#366 = VECTOR ( 'NONE', #12284, 1000.000000000000000 ) ;
#367 = LINE ( 'NONE', #8152, #5578 ) ;
#368 = CYLINDRICAL_SURFACE ( 'NONE', #956, 10.72500000000000142 ) ;
#369 = MECHANICAL_DESIGN_GEOMETRIC_PRESENTATION_REPRESENTATION (  '', ( #7806 ), #10136 ) ;
#370 = DIRECTION ( 'NONE',  ( -1.000000000000000000, 0.000000000000000000, 0.000000000000000000 ) ) ;
#371 = EDGE_CURVE ( 'NONE', #10087, #1904, #448, .T. ) ;
#372 = ORIENTED_EDGE ( 'NONE', *, *, #10389, .T. ) ;
#373 = CIRCLE ( 'NONE', #6200, 2.649999999999985700 ) ;
#374 = AXIS2_PLACEMENT_3D ( 'NONE', #11907, #9513, #3997 ) ;
#375 = CARTESIAN_POINT ( 'NONE',  ( 132.4999999999999432, -56.99999999999997158, -180.0000000000000000 ) ) ;
#376 = PLANE ( 'NONE',  #9014 ) ;
#377 = DIRECTION ( 'NONE',  ( 1.000000000000000000, 0.000000000000000000, 0.000000000000000000 ) ) ;
#378 = DIRECTION ( 'NONE',  ( 0.000000000000000000, 3.490239007934759657E-15, -1.000000000000000000 ) ) ;
#379 = ORIENTED_EDGE ( 'NONE', *, *, #6538, .T. ) ;
#380 = VECTOR ( 'NONE', #10926, 1000.000000000000000 ) ;
#381 = DIRECTION ( 'NONE',  ( 0.000000000000000000, 0.000000000000000000, -1.000000000000000000 ) ) ;
#382 = CARTESIAN_POINT ( 'NONE',  ( 2.740000000000000213, -0.5150000000000034550, 0.9838866223909983333 ) ) ;
#383 = ADVANCED_FACE ( 'NONE', ( #52 ), #4580, .F. ) ;
#384 = ORIENTED_EDGE ( 'NONE', *, *, #3098, .T. ) ;
#385 = DIRECTION ( 'NONE',  ( -1.000000000000000000, 0.000000000000000000, 0.000000000000000000 ) ) ;
#386 = VECTOR ( 'NONE', #10609, 1000.000000000000000 ) ;
#387 = CARTESIAN_POINT ( 'NONE',  ( 2.500000000000000000, -2.357898499370432610, 3.252606517456513302E-15 ) ) ;
#388 = FILL_AREA_STYLE_COLOUR ( '', #10338 ) ;
#389 = CARTESIAN_POINT ( 'NONE',  ( 0.000000000000000000, 0.000000000000000000, -0.2800830152838844622 ) ) ;
#390 = CARTESIAN_POINT ( 'NONE',  ( 302.6499999999999204, -95.00000000000008527, -169.9999999999999716 ) ) ;
#391 = CARTESIAN_POINT ( 'NONE',  ( 134.5000000000000000, -95.00000000000008527, -190.0000000000000000 ) ) ;
#392 = VECTOR ( 'NONE', #9688, 1000.000000000000000 ) ;
#393 = DIRECTION ( 'NONE',  ( 0.000000000000000000, 0.000000000000000000, 1.000000000000000000 ) ) ;
#394 = ADVANCED_FACE ( 'NONE', ( #11247 ), #10594, .F. ) ;
#395 = ORIENTED_EDGE ( 'NONE', *, *, #13834, .T. ) ;
#396 = ORIENTED_EDGE ( 'NONE', *, *, #10733, .F. ) ;
#397 = CARTESIAN_POINT ( 'NONE',  ( 82.99999999999998579, -8.660254037844389075, 200.0000000000000000 ) ) ;
#398 = EDGE_LOOP ( 'NONE', ( #3253, #13729, #3961, #12497 ) ) ;
#399 = CARTESIAN_POINT ( 'NONE',  ( 132.4999999999999716, 45.00000000000001421, 10.00000000000000000 ) ) ;
#400 =( REPRESENTATION_RELATIONSHIP ('NONE','NONE', #11251, #11637 ) REPRESENTATION_RELATIONSHIP_WITH_TRANSFORMATION ( #6106 )SHAPE_REPRESENTATION_RELATIONSHIP( ) );
#401 = ORIENTED_EDGE ( 'NONE', *, *, #3300, .T. ) ;
#402 = DIRECTION ( 'NONE',  ( -0.5000000000000051070, 1.060575238724903217E-16, -0.8660254037844355990 ) ) ;
#403 = ORIENTED_EDGE ( 'NONE', *, *, #10858, .T. ) ;
#404 = CIRCLE ( 'NONE', #11796, 0.2000000000000000944 ) ;
#405 = DIRECTION ( 'NONE',  ( 0.000000000000000000, 0.000000000000000000, -1.000000000000000000 ) ) ;
#406 = PRODUCT_DEFINITION_SHAPE ( 'NONE', 'NONE',  #14324 ) ;
#407 = DIRECTION ( 'NONE',  ( -1.000000000000000000, -0.000000000000000000, -0.000000000000000000 ) ) ;
#408 = ORIENTED_EDGE ( 'NONE', *, *, #12527, .T. ) ;
#409 = FACE_BOUND ( 'NONE', #9655, .T. ) ;
#410 = CARTESIAN_POINT ( 'NONE',  ( -30.00000000000002842, 15.00000000000000000, 205.0000000000000284 ) ) ;
#411 = FILL_AREA_STYLE_COLOUR ( '', #13957 ) ;
#412 = CARTESIAN_POINT ( 'NONE',  ( 140.0000000000000000, -75.00000000000008527, 186.2999999999999829 ) ) ;
#413 = ADVANCED_FACE ( 'NONE', ( #5943 ), #5008, .F. ) ;
#414 = PRODUCT_CONTEXT ( 'NONE', #12033, 'mechanical' ) ;
#415 = FACE_OUTER_BOUND ( 'NONE', #2522, .T. ) ;
#416 = ADVANCED_FACE ( 'NONE', ( #1651, #7249 ), #6159, .T. ) ;
#417 = VERTEX_POINT ( 'NONE', #3915 ) ;
#418 = AXIS2_PLACEMENT_3D ( 'NONE', #4704, #7151, #1554 ) ;
#419 = FACE_BOUND ( 'NONE', #9154, .T. ) ;
#420 = ORIENTED_EDGE ( 'NONE', *, *, #110, .F. ) ;
#421 = DIRECTION ( 'NONE',  ( 0.8949343913984706411, -0.4461977533473793223, 7.082407382381129037E-17 ) ) ;
#422 = ORIENTED_EDGE ( 'NONE', *, *, #251, .T. ) ;
#423 = DIRECTION ( 'NONE',  ( -0.7071067811865306973, 8.659560562355138702E-17, -0.7071067811865643371 ) ) ;
#424 = ORIENTED_EDGE ( 'NONE', *, *, #1321, .T. ) ;
#425 = LINE ( 'NONE', #10396, #7577 ) ;
#426 = ADVANCED_FACE ( 'NONE', ( #13912 ), #3987, .F. ) ;
#427 = DIRECTION ( 'NONE',  ( -1.000000000000000000, 0.000000000000000000, 0.000000000000000000 ) ) ;
#428 = CARTESIAN_POINT ( 'NONE',  ( 0.000000000000000000, 1.178949249685218525, 2.041999999999999371 ) ) ;
#429 = AXIS2_PLACEMENT_3D ( 'NONE', #11798, #3965, #8601 ) ;
#430 = DIRECTION ( 'NONE',  ( -0.000000000000000000, -0.000000000000000000, 1.000000000000000000 ) ) ;
#431 = AXIS2_PLACEMENT_3D ( 'NONE', #11953, #12886, #4331 ) ;
#432 = AXIS2_PLACEMENT_3D ( 'NONE', #6019, #1877, #3778 ) ;
#433 = CARTESIAN_POINT ( 'NONE',  ( 0.000000000000000000, 2.357898499370433054, -1.951563910473907981E-15 ) ) ;
#434 = EDGE_CURVE ( 'NONE', #8157, #4114, #1575, .T. ) ;
#435 = DIRECTION ( 'NONE',  ( 0.000000000000000000, 0.000000000000000000, 1.000000000000000000 ) ) ;
#436 = COLOUR_RGB ( '',1.000000000000000000, 0.9490196078431372140, 0.9098039215686274384 ) ;
#437 = ORIENTED_EDGE ( 'NONE', *, *, #7135, .F. ) ;
#438 = ORIENTED_EDGE ( 'NONE', *, *, #6313, .F. ) ;
#439 =( NAMED_UNIT ( * ) PLANE_ANGLE_UNIT ( ) SI_UNIT ( $, .RADIAN. ) );
#440 = VECTOR ( 'NONE', #5647, 1000.000000000000000 ) ;
#441 = LINE ( 'NONE', #4910, #14145 ) ;
#442 = DIRECTION ( 'NONE',  ( -1.000000000000000000, 0.000000000000000000, 0.000000000000000000 ) ) ;
#443 = EDGE_CURVE ( 'NONE', #12712, #546, #11238, .T. ) ;
#444 = SURFACE_STYLE_FILL_AREA ( #13745 ) ;
#445 = ORIENTED_EDGE ( 'NONE', *, *, #2431, .F. ) ;
#446 = ADVANCED_FACE ( 'NONE', ( #13984, #8328 ), #12831, .F. ) ;
#447 = CIRCLE ( 'NONE', #4421, 2.100000000000000089 ) ;
#448 = B_SPLINE_CURVE_WITH_KNOTS ( 'NONE', 3,
 ( #117, #8932, #1150, #13343 ),
 .UNSPECIFIED., .F., .F.,
 ( 4, 4 ),
 ( 0.001586480563516618056, 0.004268227385920363680 ),
 .UNSPECIFIED. ) ;
#449 = LINE ( 'NONE', #13747, #10932 ) ;
#450 = ADVANCED_FACE ( 'NONE', ( #1804 ), #8183, .F. ) ;
#451 = PLANE ( 'NONE',  #2762 ) ;
#452 = DIRECTION ( 'NONE',  ( 1.000000000000000000, 0.000000000000000000, 0.000000000000000000 ) ) ;
#453 = AXIS2_PLACEMENT_3D ( 'NONE', #6130, #4839, #11360 ) ;
#454 = DIRECTION ( 'NONE',  ( 1.000000000000000000, 0.000000000000000000, 0.000000000000000000 ) ) ;
#455 = CIRCLE ( 'NONE', #13681, 0.2000000000000022593 ) ;
#456 = ORIENTED_EDGE ( 'NONE', *, *, #9949, .T. ) ;
#457 = DIRECTION ( 'NONE',  ( 0.000000000000000000, 0.000000000000000000, -1.000000000000000000 ) ) ;
#458 = FACE_OUTER_BOUND ( 'NONE', #13462, .T. ) ;
#459 = CIRCLE ( 'NONE', #14158, 2.500000000000002220 ) ;
#460 = ORIENTED_EDGE ( 'NONE', *, *, #9965, .F. ) ;
#461 = CARTESIAN_POINT ( 'NONE',  ( 2.500000000000000000, -2.357898499370432610, 3.252606517456513302E-15 ) ) ;
#462 =( GEOMETRIC_REPRESENTATION_CONTEXT ( 3 ) GLOBAL_UNCERTAINTY_ASSIGNED_CONTEXT ( ( #11763 ) ) GLOBAL_UNIT_ASSIGNED_CONTEXT ( ( #13639, #8054, #9372 ) ) REPRESENTATION_CONTEXT ( 'NONE', 'WORKASPACE' ) );
#463 = DIRECTION ( 'NONE',  ( -1.000000000000000000, 0.000000000000000000, 0.000000000000000000 ) ) ;
#464 = CARTESIAN_POINT ( 'NONE',  ( 53.33333333333330017, -20.00000000000000000, -222.5000000000000853 ) ) ;
#465 = FACE_BOUND ( 'NONE', #5251, .T. ) ;
#466 = CARTESIAN_POINT ( 'NONE',  ( 0.06760930072668842883, -0.5149999999999961275, -0.9010842325122929708 ) ) ;
#467 = CARTESIAN_POINT ( 'NONE',  ( 4.999999999999999112, 8.660254037844390851, 210.0000000000000000 ) ) ;
#468 = SURFACE_SIDE_STYLE ('',( #3620 ) ) ;
#469 = CARTESIAN_POINT ( 'NONE',  ( 307.4999999999999432, 45.00000000000001421, 10.00000000000000000 ) ) ;
#470 = ITEM_DEFINED_TRANSFORMATION ( 'NONE', 'NONE', #13712,  #14039 ) ;
#471 = VECTOR ( 'NONE', #1834, 1000.000000000000000 ) ;
#472 = ADVANCED_FACE ( 'NONE', ( #7101 ), #8920, .F. ) ;
#473 = AXIS2_PLACEMENT_3D ( 'NONE', #9647, #5162, #2982 ) ;
#474 = ORIENTED_EDGE ( 'NONE', *, *, #10554, .T. ) ;
#475 = DIRECTION ( 'NONE',  ( -1.000000000000000000, 0.000000000000000000, 0.000000000000000000 ) ) ;
#476 = COLOUR_RGB ( '',1.000000000000000000, 0.9490196078431372140, 0.9098039215686274384 ) ;
#477 = EDGE_LOOP ( 'NONE', ( #11769, #9508 ) ) ;
#478 = CARTESIAN_POINT ( 'NONE',  ( 2.691179338796023329E-15, 4.647089433458991614, -3.572167766733753691 ) ) ;
#479 = CARTESIAN_POINT ( 'NONE',  ( -299.9999999999999432, -95.00000000000008527, 354.1421356237308942 ) ) ;
#480 = EDGE_LOOP ( 'NONE', ( #9749, #7641, #121, #4547, #3837, #13911, #3499, #11062 ) ) ;
#481 = CARTESIAN_POINT ( 'NONE',  ( 219.9999999999999716, -20.00000000000000000, -222.5000000000000853 ) ) ;
#482 = ORIENTED_EDGE ( 'NONE', *, *, #7284, .T. ) ;
#483 = PLANE ( 'NONE',  #11041 ) ;
#484 = CARTESIAN_POINT ( 'NONE',  ( 0.000000000000000000, 0.000000000000000000, -4.974599999999998801 ) ) ;
#486 = VERTEX_POINT ( 'NONE', #1503 ) ;
#485 = VECTOR ( 'NONE', #5913, 1000.000000000000000 ) ;
#487 = FACE_BOUND ( 'NONE', #5303, .T. ) ;
#488 = CARTESIAN_POINT ( 'NONE',  ( 4.999999999999997335, -8.660254037844389075, -200.0000000000000000 ) ) ;
#489 = AXIS2_PLACEMENT_3D ( 'NONE', #301, #5995, #1412 ) ;
#490 = SURFACE_STYLE_USAGE ( .BOTH. , #3852 ) ;
#491 =( GEOMETRIC_REPRESENTATION_CONTEXT ( 3 ) GLOBAL_UNCERTAINTY_ASSIGNED_CONTEXT ( ( #7550 ) ) GLOBAL_UNIT_ASSIGNED_CONTEXT ( ( #9395, #10194, #4976 ) ) REPRESENTATION_CONTEXT ( 'NONE', 'WORKASPACE' ) );
#492 = VECTOR ( 'NONE', #6472, 1000.000000000000114 ) ;
#493 = SHAPE_DEFINITION_REPRESENTATION ( #2167, #7730 ) ;
#494 = DIRECTION ( 'NONE',  ( -0.000000000000000000, -0.000000000000000000, 1.000000000000000000 ) ) ;
#495 = EDGE_LOOP ( 'NONE', ( #2805, #3128, #6532, #2703 ) ) ;
#496 = ORIENTED_EDGE ( 'NONE', *, *, #11704, .F. ) ;
#497 = TOROIDAL_SURFACE ( 'NONE', #7925, 13.29999999999999893, 0.2000000000000027034 ) ;
#498 = VERTEX_POINT ( 'NONE', #10666 ) ;
#499 = DIRECTION ( 'NONE',  ( 0.000000000000000000, 0.000000000000000000, -1.000000000000000000 ) ) ;
#500 = PRODUCT_DEFINITION_FORMATION_WITH_SPECIFIED_SOURCE ( 'ANY', '', #10165, .NOT_KNOWN. ) ;
#501 = EDGE_LOOP ( 'NONE', ( #3700, #503, #1246, #7982 ) ) ;
#502 = DIRECTION ( 'NONE',  ( -1.000000000000000000, 0.000000000000000000, -0.000000000000000000 ) ) ;
#503 = ORIENTED_EDGE ( 'NONE', *, *, #10674, .T. ) ;
#504 = EDGE_CURVE ( 'NONE', #1416, #12143, #787, .T. ) ;
#505 = DIRECTION ( 'NONE',  ( 0.000000000000000000, 1.000000000000000000, 0.000000000000000000 ) ) ;
#506 = ADVANCED_FACE ( 'NONE', ( #12686 ), #13842, .F. ) ;
#507 = LINE ( 'NONE', #9385, #4377 ) ;
#508 = FACE_OUTER_BOUND ( 'NONE', #3187, .T. ) ;
#509 = CIRCLE ( 'NONE', #8650, 9.999999999999980460 ) ;
#510 = CARTESIAN_POINT ( 'NONE',  ( -25.39999999999996305, 0.000000000000000000, 2.500000000000000000 ) ) ;
#511 = DIRECTION ( 'NONE',  ( -1.000000000000000000, 0.000000000000000000, 0.000000000000000000 ) ) ;
#512 = DIRECTION ( 'NONE',  ( -1.000000000000000000, -0.000000000000000000, -0.000000000000000000 ) ) ;
#513 = EDGE_LOOP ( 'NONE', ( #5449, #4903, #1270 ) ) ;
#514 = VERTEX_POINT ( 'NONE', #397 ) ;
#515 =( LENGTH_UNIT ( ) NAMED_UNIT ( * ) SI_UNIT ( .MILLI., .METRE. ) );
#516 = CARTESIAN_POINT ( 'NONE',  ( 0.6507732100473444525, -4.243078065514795050, -0.2236248678334952777 ) ) ;
#517 = EDGE_CURVE ( 'NONE', #10395, #2635, #95, .T. ) ;
#518 = CARTESIAN_POINT ( 'NONE',  ( 2.500000000000000000, 2.357898499370433054, -1.951563910473907981E-15 ) ) ;
#519 = PRODUCT_RELATED_PRODUCT_CATEGORY ( 'part', '', ( #59 ) ) ;
#520 = CARTESIAN_POINT ( 'NONE',  ( -144.9999999999999432, -105.0000000000000853, 40.00000000000000000 ) ) ;
#521 = ORIENTED_EDGE ( 'NONE', *, *, #4268, .F. ) ;
#522 = CARTESIAN_POINT ( 'NONE',  ( 2.500000000000000000, -1.178949249685218303, -2.041999999999998039 ) ) ;
#523 = DIRECTION ( 'NONE',  ( 1.000000000000000000, 0.000000000000000000, 0.000000000000000000 ) ) ;
#524 = CARTESIAN_POINT ( 'NONE',  ( 134.9999999999999716, 45.00000000000001421, 145.0000000000000000 ) ) ;
#525 = DIRECTION ( 'NONE',  ( 1.000000000000000000, 0.000000000000000000, 0.000000000000000000 ) ) ;
#526 = VECTOR ( 'NONE', #13201, 1000.000000000000000 ) ;
#527 = LINE ( 'NONE', #11178, #7784 ) ;
#528 = ADVANCED_FACE ( 'NONE', ( #2680 ), #11531, .F. ) ;
#529 = ADVANCED_FACE ( 'NONE', ( #4940 ), #3828, .F. ) ;
#530 = EDGE_CURVE ( 'NONE', #11552, #6716, #8218, .T. ) ;
#531 = EDGE_CURVE ( 'NONE', #10688, #3025, #6522, .T. ) ;
#532 = VERTEX_POINT ( 'NONE', #10807 ) ;
#533 = CYLINDRICAL_SURFACE ( 'NONE', #8092, 5.500000000000005329 ) ;
#534 = PRODUCT_DEFINITION_SHAPE ( 'NONE', 'NONE',  #14373 ) ;
#535 = DIRECTION ( 'NONE',  ( 0.000000000000000000, 0.000000000000000000, -1.000000000000000000 ) ) ;
#536 = ORIENTED_EDGE ( 'NONE', *, *, #14163, .F. ) ;
#537 = CARTESIAN_POINT ( 'NONE',  ( 347.0000000000000000, 8.660254037844390851, 199.9990000000000236 ) ) ;
#538 = SURFACE_STYLE_FILL_AREA ( #13829 ) ;
#539 =( REPRESENTATION_RELATIONSHIP ('NONE','NONE', #11251, #5332 ) REPRESENTATION_RELATIONSHIP_WITH_TRANSFORMATION ( #7958 )SHAPE_REPRESENTATION_RELATIONSHIP( ) );
#540 = CARTESIAN_POINT ( 'NONE',  ( 203.5000000000000000, -85.00000000000007105, 55.00000000000001421 ) ) ;
#541 = CARTESIAN_POINT ( 'NONE',  ( 299.9999999999999432, -75.00000000000008527, -186.2999999999999829 ) ) ;
#542 = CARTESIAN_POINT ( 'NONE',  ( -299.9999999999999432, -75.00000000000008527, 354.1421356237308942 ) ) ;
#543 = LINE ( 'NONE', #10288, #10586 ) ;
#544 = AXIS2_PLACEMENT_3D ( 'NONE', #926, #9879, #13212 ) ;
#545 = DIRECTION ( 'NONE',  ( 0.000000000000000000, 0.000000000000000000, 1.000000000000000000 ) ) ;
#546 = VERTEX_POINT ( 'NONE', #7599 ) ;
#547 = DIRECTION ( 'NONE',  ( 0.000000000000000000, -0.000000000000000000, 1.000000000000000000 ) ) ;
#548 = ORIENTED_EDGE ( 'NONE', *, *, #9525, .F. ) ;
#549 = DIRECTION ( 'NONE',  ( -1.000000000000000000, 0.000000000000000000, -0.000000000000000000 ) ) ;
#550 = CARTESIAN_POINT ( 'NONE',  ( 7.345657149124340535, -9.419606183588304946E-15, 1.312408941150045472 ) ) ;
#551 = AXIS2_PLACEMENT_3D ( 'NONE', #694, #9431, #11675 ) ;
#552 = AXIS2_PLACEMENT_3D ( 'NONE', #1164, #6764, #11129 ) ;
#553 = EDGE_LOOP ( 'NONE', ( #2491, #10447 ) ) ;
#554 = DIRECTION ( 'NONE',  ( 0.000000000000000000, 0.000000000000000000, 1.000000000000000000 ) ) ;
#555 = ORIENTED_EDGE ( 'NONE', *, *, #6914, .F. ) ;
#556 = DIRECTION ( 'NONE',  ( 1.000000000000000000, 0.000000000000000000, 0.000000000000000000 ) ) ;
#557 = CARTESIAN_POINT ( 'NONE',  ( -4.000000000000000000, 0.7924765000094600165, -0.05906175389889745803 ) ) ;
#558 = ORIENTED_EDGE ( 'NONE', *, *, #6357, .F. ) ;
#559 = FACE_BOUND ( 'NONE', #6521, .T. ) ;
#560 = ADVANCED_FACE ( 'NONE', ( #13188 ), #11821, .F. ) ;
#561 = DIRECTION ( 'NONE',  ( -1.000000000000000000, -0.000000000000000000, -0.000000000000000000 ) ) ;
#562 = DIRECTION ( 'NONE',  ( 0.000000000000000000, 0.000000000000000000, 1.000000000000000000 ) ) ;
#563 = SHAPE_DEFINITION_REPRESENTATION ( #6804, #2740 ) ;
#564 = FACE_OUTER_BOUND ( 'NONE', #5808, .T. ) ;
#565 = AXIS2_PLACEMENT_3D ( 'NONE', #12068, #10768, #6552 ) ;
#566 = VERTEX_POINT ( 'NONE', #14267 ) ;
#567 = CIRCLE ( 'NONE', #11715, 5.500000000000005329 ) ;
#568 = VERTEX_POINT ( 'NONE', #766 ) ;
#569 = ORIENTED_EDGE ( 'NONE', *, *, #1110, .T. ) ;
#570 = ORIENTED_EDGE ( 'NONE', *, *, #8444, .F. ) ;
#571 = DIRECTION ( 'NONE',  ( -0.000000000000000000, -0.000000000000000000, -1.000000000000000000 ) ) ;
#572 = ORIENTED_EDGE ( 'NONE', *, *, #8259, .T. ) ;
#573 = DIRECTION ( 'NONE',  ( -0.000000000000000000, -0.000000000000000000, -1.000000000000000000 ) ) ;
#574 = VERTEX_POINT ( 'NONE', #11897 ) ;
#575 = DIRECTION ( 'NONE',  ( 1.000000000000000000, 7.304098846218135653E-17, -0.000000000000000000 ) ) ;
#576 = CIRCLE ( 'NONE', #10566, 12.44999999999999929 ) ;
#577 = DIRECTION ( 'NONE',  ( -1.000000000000000000, 0.000000000000000000, 0.000000000000000000 ) ) ;
#578 = CARTESIAN_POINT ( 'NONE',  ( 0.000000000000000000, -0.5150000000000080069, 2.349999999999998312 ) ) ;
#579 = DIRECTION ( 'NONE',  ( 0.000000000000000000, 0.000000000000000000, -1.000000000000000000 ) ) ;
#580 = CARTESIAN_POINT ( 'NONE',  ( 142.6500000000000057, -75.00000000000008527, 190.0000000000000000 ) ) ;
#581 = CARTESIAN_POINT ( 'NONE',  ( -30.00000000000002842, -25.00000000000000000, -190.0000000000000000 ) ) ;
#582 = VECTOR ( 'NONE', #10152, 1000.000000000000000 ) ;
#583 = ORIENTED_EDGE ( 'NONE', *, *, #10908, .F. ) ;
#584 = EDGE_CURVE ( 'NONE', #2928, #10867, #1475, .T. ) ;
#585 = ORIENTED_EDGE ( 'NONE', *, *, #10780, .T. ) ;
#586 = VECTOR ( 'NONE', #11904, 1000.000000000000000 ) ;
#588 = CARTESIAN_POINT ( 'NONE',  ( 0.000000000000000000, -2.357898499370432166, 3.035766082959412415E-15 ) ) ;
#587 = AXIS2_PLACEMENT_3D ( 'NONE', #14240, #5547, #9979 ) ;
#589 = ORIENTED_EDGE ( 'NONE', *, *, #5616, .T. ) ;
#590 = LINE ( 'NONE', #1845, #7331 ) ;
#591 = CARTESIAN_POINT ( 'NONE',  ( 0.000000000000000000, 0.000000000000000000, 0.000000000000000000 ) ) ;
#592 = PLANE ( 'NONE',  #11528 ) ;
#593 = AXIS2_PLACEMENT_3D ( 'NONE', #467, #9356, #3452 ) ;
#594 = ORIENTED_EDGE ( 'NONE', *, *, #14027, .F. ) ;
#595 = CIRCLE ( 'NONE', #10589, 2.649999999999985700 ) ;
#596 = VECTOR ( 'NONE', #756, 999.9999999999998863 ) ;
#597 = DIRECTION ( 'NONE',  ( -1.000000000000000000, -0.000000000000000000, -0.000000000000000000 ) ) ;
#598 = AXIS2_PLACEMENT_3D ( 'NONE', #11123, #1157, #11993 ) ;
#599 = CARTESIAN_POINT ( 'NONE',  ( 0.000000000000000000, 0.000000000000000000, 186.0000000000000000 ) ) ;
#600 = DIRECTION ( 'NONE',  ( -1.000000000000000000, 0.000000000000000000, 0.000000000000000000 ) ) ;
#601 = CIRCLE ( 'NONE', #4808, 5.500000000000005329 ) ;
#602 = CARTESIAN_POINT ( 'NONE',  ( 0.000000000000000000, 0.000000000000000000, -0.3080913168122742518 ) ) ;
#603 = EDGE_CURVE ( 'NONE', #5710, #9112, #7307, .T. ) ;
#604 = DIRECTION ( 'NONE',  ( 0.000000000000000000, 0.000000000000000000, -1.000000000000000000 ) ) ;
#605 = APPLICATION_CONTEXT ( 'automotive_design' ) ;
#606 = ORIENTED_EDGE ( 'NONE', *, *, #1377, .T. ) ;
#607 = CARTESIAN_POINT ( 'NONE',  ( 53.33333333333330017, -20.00000000000000000, 225.1500000000000625 ) ) ;
#608 = AXIS2_PLACEMENT_3D ( 'NONE', #4664, #202, #3506 ) ;
#609 = LINE ( 'NONE', #2598, #1621 ) ;
#610 = CIRCLE ( 'NONE', #14302, 12.77500000000000036 ) ;
#611 = VERTEX_POINT ( 'NONE', #9793 ) ;
#612 = CARTESIAN_POINT ( 'NONE',  ( 2.500000000000000000, 2.357898499370433054, -1.951563910473907981E-15 ) ) ;
#613 = EDGE_CURVE ( 'NONE', #4926, #11608, #3124, .T. ) ;
#614 = EDGE_CURVE ( 'NONE', #1243, #10967, #14200, .T. ) ;
#615 =( NAMED_UNIT ( * ) PLANE_ANGLE_UNIT ( ) SI_UNIT ( $, .RADIAN. ) );
#616 = VECTOR ( 'NONE', #713, 1000.000000000000000 ) ;
#617 = DIRECTION ( 'NONE',  ( -0.000000000000000000, -0.000000000000000000, 1.000000000000000000 ) ) ;
#618 = ADVANCED_FACE ( 'NONE', ( #13049 ), #6593, .T. ) ;
#619 = CARTESIAN_POINT ( 'NONE',  ( 2.500000000000000000, 1.768423874527824902, 1.020999999999999019 ) ) ;
#620 = AXIS2_PLACEMENT_3D ( 'NONE', #2454, #1137, #8922 ) ;
#621 = DIRECTION ( 'NONE',  ( -0.000000000000000000, -0.000000000000000000, 1.000000000000000000 ) ) ;
#622 = FACE_BOUND ( 'NONE', #8043, .T. ) ;
#623 = FILL_AREA_STYLE_COLOUR ( '', #476 ) ;
#624 = FACE_OUTER_BOUND ( 'NONE', #10767, .T. ) ;
#625 = CONTEXT_DEPENDENT_SHAPE_REPRESENTATION ( #11693, #12963 ) ;
#626 = CIRCLE ( 'NONE', #2277, 2.649999999999985700 ) ;
#627 = EDGE_LOOP ( 'NONE', ( #3, #5676 ) ) ;
#628 = DIRECTION ( 'NONE',  ( 0.000000000000000000, 0.000000000000000000, -1.000000000000000000 ) ) ;
#629 = ORIENTED_EDGE ( 'NONE', *, *, #10325, .T. ) ;
#630 = FACE_OUTER_BOUND ( 'NONE', #8470, .T. ) ;
#631 = LINE ( 'NONE', #3992, #11133 ) ;
#632 = ORIENTED_EDGE ( 'NONE', *, *, #9818, .T. ) ;
#633 = CARTESIAN_POINT ( 'NONE',  ( 386.6666666666666288, -14.99999999999999822, 219.8500000000001080 ) ) ;
#634 = VERTEX_POINT ( 'NONE', #11963 ) ;
#635 = LINE ( 'NONE', #10377, #5692 ) ;
#636 =( GEOMETRIC_REPRESENTATION_CONTEXT ( 3 ) GLOBAL_UNCERTAINTY_ASSIGNED_CONTEXT ( ( #7199 ) ) GLOBAL_UNIT_ASSIGNED_CONTEXT ( ( #9242, #8209, #12578 ) ) REPRESENTATION_CONTEXT ( 'NONE', 'WORKASPACE' ) );
#637 = DIRECTION ( 'NONE',  ( -1.000000000000000000, -0.000000000000000000, -0.000000000000000000 ) ) ;
#638 = EDGE_LOOP ( 'NONE', ( #7545, #6355, #6179, #9350 ) ) ;
#639 = ADVANCED_FACE ( 'NONE', ( #12036 ), #6380, .T. ) ;
#640 = FACE_OUTER_BOUND ( 'NONE', #1038, .T. ) ;
#641 = CARTESIAN_POINT ( 'NONE',  ( 134.5000000000000000, -95.00000000000008527, 186.2999999999999829 ) ) ;
#642 = FILL_AREA_STYLE_COLOUR ( '', #2323 ) ;
#643 = ADVANCED_FACE ( 'NONE', ( #9643 ), #839, .F. ) ;
#644 = APPLICATION_PROTOCOL_DEFINITION ( 'draft international standard', 'automotive_design', 1998, #13313 ) ;
#645 = DIRECTION ( 'NONE',  ( 0.000000000000000000, 0.000000000000000000, 1.000000000000000000 ) ) ;
#646 = ORIENTED_EDGE ( 'NONE', *, *, #7816, .F. ) ;
#647 = EDGE_LOOP ( 'NONE', ( #6758, #1729, #6097, #8404 ) ) ;
#648 = LINE ( 'NONE', #5110, #4286 ) ;
#649 = VERTEX_POINT ( 'NONE', #8693 ) ;
#650 = CARTESIAN_POINT ( 'NONE',  ( 2.171643655288379993, -3.365003104552334978, -1.195831703456429434E-14 ) ) ;
#651 = AXIS2_PLACEMENT_3D ( 'NONE', #4786, #10439, #3836 ) ;
#652 = ORIENTED_EDGE ( 'NONE', *, *, #7099, .T. ) ;
#653 = FACE_OUTER_BOUND ( 'NONE', #14300, .T. ) ;
#654 = ORIENTED_EDGE ( 'NONE', *, *, #11946, .F. ) ;
#655 = CARTESIAN_POINT ( 'NONE',  ( 0.000000000000000000, 0.000000000000000000, 186.0000000000000000 ) ) ;
#656 = CARTESIAN_POINT ( 'NONE',  ( -20.63749999999999574, 0.000000000000000000, 0.000000000000000000 ) ) ;
#657 = FACE_OUTER_BOUND ( 'NONE', #3143, .T. ) ;
#658 = DIRECTION ( 'NONE',  ( -1.000000000000000000, 0.000000000000000000, 0.000000000000000000 ) ) ;
#659 =( LENGTH_UNIT ( ) NAMED_UNIT ( * ) SI_UNIT ( .MILLI., .METRE. ) );
#660 = VECTOR ( 'NONE', #9403, 1000.000000000000000 ) ;
#661 = DIRECTION ( 'NONE',  ( 0.000000000000000000, 1.000000000000000000, 3.280956645156627724E-15 ) ) ;
#662 = PRODUCT_DEFINITION_SHAPE ( 'NONE', 'NONE',  #14379 ) ;
#663 = VERTEX_POINT ( 'NONE', #2017 ) ;
#664 = ORIENTED_EDGE ( 'NONE', *, *, #6928, .F. ) ;
#665 = EDGE_CURVE ( 'NONE', #10366, #9474, #11020, .T. ) ;
#666 = DIRECTION ( 'NONE',  ( -1.000000000000000000, -0.000000000000000000, -0.000000000000000000 ) ) ;
#667 = ORIENTED_EDGE ( 'NONE', *, *, #11104, .F. ) ;
#668 = CARTESIAN_POINT ( 'NONE',  ( 297.3499999999999659, -75.00000000000008527, 190.0000000000000000 ) ) ;
#669 = AXIS2_PLACEMENT_3D ( 'NONE', #13246, #4259, #10035 ) ;
#670 = CARTESIAN_POINT ( 'NONE',  ( 53.33333333333330017, -20.00000000000000000, 219.8500000000001080 ) ) ;
#671 = ORIENTED_EDGE ( 'NONE', *, *, #14160, .F. ) ;
#672=STYLED_ITEM('',(#14403),#3882);
#673 = PLANE ( 'NONE',  #8840 ) ;
#674 = DIRECTION ( 'NONE',  ( 0.000000000000000000, 0.000000000000000000, -1.000000000000000000 ) ) ;
#675 = DIRECTION ( 'NONE',  ( 6.123233995736766036E-17, -1.000000000000000000, 0.000000000000000000 ) ) ;
#676 = CARTESIAN_POINT ( 'NONE',  ( 0.000000000000000000, 0.000000000000000000, -25.03750572909317285 ) ) ;
#677 = ORIENTED_EDGE ( 'NONE', *, *, #85, .T. ) ;
#678 = VERTEX_POINT ( 'NONE', #7669 ) ;
#679 = CARTESIAN_POINT ( 'NONE',  ( 359.9999999999997726, 35.00000000000002842, 0.000000000000000000 ) ) ;
#680 = AXIS2_PLACEMENT_3D ( 'NONE', #9201, #13616, #5933 ) ;
#681 = DIRECTION ( 'NONE',  ( 0.000000000000000000, 0.000000000000000000, -1.000000000000000000 ) ) ;
#682 = VERTEX_POINT ( 'NONE', #2166 ) ;
#684 = ADVANCED_FACE ( 'NONE', ( #12904 ), #1050, .F. ) ;
#683 = DIRECTION ( 'NONE',  ( -0.7071067811865369146, 8.659560562355062281E-17, -0.7071067811865582309 ) ) ;
#685 = EDGE_CURVE ( 'NONE', #13286, #10688, #9930, .T. ) ;
#686 = CIRCLE ( 'NONE', #9763, 2.500000000000000444 ) ;
#687 = CARTESIAN_POINT ( 'NONE',  ( 386.6666666666666288, -20.00000000000000000, -225.1500000000000625 ) ) ;
#688 = DIRECTION ( 'NONE',  ( 0.000000000000000000, -1.000000000000000000, 0.000000000000000000 ) ) ;
#689 = LINE ( 'NONE', #14053, #13631 ) ;
#690 = AXIS2_PLACEMENT_3D ( 'NONE', #8292, #2793, #13735 ) ;
#691 = DIRECTION ( 'NONE',  ( 1.000000000000000000, 0.000000000000000000, 0.000000000000000000 ) ) ;
#692 = EDGE_LOOP ( 'NONE', ( #5949, #6381, #4636, #10880 ) ) ;
#693 = EDGE_CURVE ( 'NONE', #6913, #7861, #567, .T. ) ;
#694 = CARTESIAN_POINT ( 'NONE',  ( 2.740000000000000213, 0.000000000000000000, 0.000000000000000000 ) ) ;
#695 = AXIS2_PLACEMENT_3D ( 'NONE', #1037, #5488, #9920 ) ;
#696 = ORIENTED_EDGE ( 'NONE', *, *, #2963, .T. ) ;
#697 = DIRECTION ( 'NONE',  ( 1.224646799147353207E-16, 1.000000000000000000, 0.000000000000000000 ) ) ;
#698 = DIRECTION ( 'NONE',  ( -1.000000000000000000, -0.000000000000000000, -0.000000000000000000 ) ) ;
#699 = ORIENTED_EDGE ( 'NONE', *, *, #13846, .F. ) ;
#700 = CARTESIAN_POINT ( 'NONE',  ( -2.000000000000001776, 0.000000000000000000, 0.000000000000000000 ) ) ;
#701 = VERTEX_POINT ( 'NONE', #8913 ) ;
#702 = MECHANICAL_DESIGN_GEOMETRIC_PRESENTATION_REPRESENTATION (  '', ( #10000 ), #9500 ) ;
#704 = EDGE_CURVE ( 'NONE', #9413, #1808, #6868, .T. ) ;
#703 = PLANE ( 'NONE',  #2931 ) ;
#705 = EDGE_CURVE ( 'NONE', #8299, #11820, #1204, .T. ) ;
#706 = CARTESIAN_POINT ( 'NONE',  ( -4.211140560182196957, -2.431303136016552013, -3.745885042887436178 ) ) ;
#707 = ORIENTED_EDGE ( 'NONE', *, *, #13975, .F. ) ;
#708 = UNCERTAINTY_MEASURE_WITH_UNIT (LENGTH_MEASURE( 1.000000000000000082E-05 ), #11198, 'distance_accuracy_value', 'NONE');
#709 = FACE_OUTER_BOUND ( 'NONE', #10738, .T. ) ;
#710 = AXIS2_PLACEMENT_3D ( 'NONE', #12147, #4322, #3386 ) ;
#711 = ADVANCED_FACE ( 'NONE', ( #4494 ), #2218, .T. ) ;
#712 = DIRECTION ( 'NONE',  ( -1.000000000000000000, 0.000000000000000000, 0.000000000000000000 ) ) ;
#713 = DIRECTION ( 'NONE',  ( 1.000000000000000000, 0.000000000000000000, 0.000000000000000000 ) ) ;
#714 = ORIENTED_EDGE ( 'NONE', *, *, #5887, .F. ) ;
#715 = ORIENTED_EDGE ( 'NONE', *, *, #13042, .T. ) ;
#716 = EDGE_CURVE ( 'NONE', #12041, #2872, #7875, .T. ) ;
#717 = EDGE_CURVE ( 'NONE', #7761, #2624, #1126, .T. ) ;
#718 = ORIENTED_EDGE ( 'NONE', *, *, #4541, .F. ) ;
#719 = ORIENTED_EDGE ( 'NONE', *, *, #8532, .T. ) ;
#720 = EDGE_CURVE ( 'NONE', #10091, #8663, #9863, .T. ) ;
#721 = CARTESIAN_POINT ( 'NONE',  ( 303.3333333333333144, -20.00000000000000000, 222.5000000000000853 ) ) ;
#722 = VERTEX_POINT ( 'NONE', #12315 ) ;
#723 = CIRCLE ( 'NONE', #11163, 10.00000000000000000 ) ;
#724 = ORIENTED_EDGE ( 'NONE', *, *, #9957, .F. ) ;
#725 = CARTESIAN_POINT ( 'NONE',  ( 259.0000000000000000, 8.660254037844390851, 199.9990000000000236 ) ) ;
#726 = ORIENTED_EDGE ( 'NONE', *, *, #8107, .T. ) ;
#727 = DIRECTION ( 'NONE',  ( 1.000000000000000000, 0.000000000000000000, 0.000000000000000000 ) ) ;
#728 = EDGE_CURVE ( 'NONE', #4230, #2998, #2381, .T. ) ;
#729 = AXIS2_PLACEMENT_3D ( 'NONE', #5568, #7596, #2162 ) ;
#730 = DIRECTION ( 'NONE',  ( 1.000000000000000000, 0.000000000000000000, 0.000000000000000000 ) ) ;
#731 =( GEOMETRIC_REPRESENTATION_CONTEXT ( 3 ) GLOBAL_UNCERTAINTY_ASSIGNED_CONTEXT ( ( #3078 ) ) GLOBAL_UNIT_ASSIGNED_CONTEXT ( ( #5611, #5743, #3573 ) ) REPRESENTATION_CONTEXT ( 'NONE', 'WORKASPACE' ) );
#732 = DIRECTION ( 'NONE',  ( -1.000000000000000000, 0.000000000000000000, -0.000000000000000000 ) ) ;
#733 = DIRECTION ( 'NONE',  ( 0.000000000000000000, 1.000000000000000000, -1.287488025362403787E-15 ) ) ;
#734 = CARTESIAN_POINT ( 'NONE',  ( 0.2500000000000002220, 5.204748896376250699E-16, -4.250000000000000000 ) ) ;
#735 = AXIS2_PLACEMENT_3D ( 'NONE', #2825, #8104, #11669 ) ;
#736 = ORIENTED_EDGE ( 'NONE', *, *, #1947, .F. ) ;
#737 = ORIENTED_EDGE ( 'NONE', *, *, #74, .T. ) ;
#738 = ORIENTED_EDGE ( 'NONE', *, *, #5484, .T. ) ;
#739 = DIRECTION ( 'NONE',  ( -0.000000000000000000, -0.000000000000000000, 1.000000000000000000 ) ) ;
#740 = CARTESIAN_POINT ( 'NONE',  ( -304.9999999999999432, -75.00000000000008527, 39.99999999999997868 ) ) ;
#741 = CYLINDRICAL_SURFACE ( 'NONE', #5392, 2.649999999999985700 ) ;
#742 = AXIS2_PLACEMENT_3D ( 'NONE', #12289, #7713, #2203 ) ;
#743 = CARTESIAN_POINT ( 'NONE',  ( 214.9999999999999716, -85.00000000000007105, 64.14213562373096522 ) ) ;
#744 = ORIENTED_EDGE ( 'NONE', *, *, #9206, .T. ) ;
#745 = CARTESIAN_POINT ( 'NONE',  ( 4.000000000000000000, 0.000000000000000000, 0.000000000000000000 ) ) ;
#746 = FACE_OUTER_BOUND ( 'NONE', #11832, .T. ) ;
#747 = EDGE_CURVE ( 'NONE', #11219, #4789, #11024, .T. ) ;
#748 = DIRECTION ( 'NONE',  ( 0.000000000000000000, 0.000000000000000000, 1.000000000000000000 ) ) ;
#749 = DIRECTION ( 'NONE',  ( 6.123233995736766036E-17, -1.000000000000000000, 0.000000000000000000 ) ) ;
#750 = DIRECTION ( 'NONE',  ( -0.000000000000000000, 1.000000000000000000, -0.000000000000000000 ) ) ;
#751 = ORIENTED_EDGE ( 'NONE', *, *, #4831, .F. ) ;
#752 = EDGE_LOOP ( 'NONE', ( #1446, #5802, #10975, #13060 ) ) ;
#753 = FACE_OUTER_BOUND ( 'NONE', #6198, .T. ) ;
#754 = DIRECTION ( 'NONE',  ( -0.000000000000000000, 0.000000000000000000, 1.000000000000000000 ) ) ;
#755 = ORIENTED_EDGE ( 'NONE', *, *, #8686, .T. ) ;
#756 = DIRECTION ( 'NONE',  ( 0.8191520442889875797, 0.000000000000000000, 0.5735764363510522656 ) ) ;
#757 = UNCERTAINTY_MEASURE_WITH_UNIT (LENGTH_MEASURE( 1.000000000000000082E-05 ), #6447, 'distance_accuracy_value', 'NONE');
#758 = EDGE_CURVE ( 'NONE', #13517, #7253, #6624, .T. ) ;
#759 =( LENGTH_UNIT ( ) NAMED_UNIT ( * ) SI_UNIT ( .MILLI., .METRE. ) );
#760 = CARTESIAN_POINT ( 'NONE',  ( 4.000000000000000000, -2.471525695159793035, -3.686886880705770864 ) ) ;
#761 = LINE ( 'NONE', #8324, #11554 ) ;
#762 =( NAMED_UNIT ( * ) SI_UNIT ( $, .STERADIAN. ) SOLID_ANGLE_UNIT ( ) );
#763 = ITEM_DEFINED_TRANSFORMATION ( 'NONE', 'NONE', #4924,  #14039 ) ;
#764 = VERTEX_POINT ( 'NONE', #2524 ) ;
#765 = EDGE_CURVE ( 'NONE', #9549, #5968, #7772, .T. ) ;
#766 = CARTESIAN_POINT ( 'NONE',  ( 0.000000000000000000, -2.357898499370432610, 3.252606517456513302E-15 ) ) ;
#767 = ORIENTED_EDGE ( 'NONE', *, *, #841, .F. ) ;
#768 = LINE ( 'NONE', #3270, #2096 ) ;
#769 = LINE ( 'NONE', #1579, #4481 ) ;
#770 = VERTEX_POINT ( 'NONE', #6803 ) ;
#771 = CARTESIAN_POINT ( 'NONE',  ( -4.197393957002303999, 0.4069871074557429025, -3.503767560748926257 ) ) ;
#772 = EDGE_LOOP ( 'NONE', ( #14040, #14210, #372, #7897 ) ) ;
#773 = CARTESIAN_POINT ( 'NONE',  ( 124.9999999999999574, -64.99999999999997158, 10.00000000000000000 ) ) ;
#774 = PRODUCT_DEFINITION_SHAPE ( 'NONE', 'NONE',  #14354 ) ;
#775 = DIRECTION ( 'NONE',  ( -1.000000000000000000, 0.000000000000000000, 0.000000000000000000 ) ) ;
#776 = VECTOR ( 'NONE', #9953, 1000.000000000000000 ) ;
#777 = ORIENTED_EDGE ( 'NONE', *, *, #7329, .T. ) ;
#778 = CARTESIAN_POINT ( 'NONE',  ( -5.000000000000000888, 8.660254037844390851, 210.0000000000000000 ) ) ;
#779 = CARTESIAN_POINT ( 'NONE',  ( 5.000000000000004441, 0.000000000000000000, 0.000000000000000000 ) ) ;
#780 = SURFACE_SIDE_STYLE ('',( #7408 ) ) ;
#781 = SURFACE_STYLE_FILL_AREA ( #10754 ) ;
#782 = CARTESIAN_POINT ( 'NONE',  ( 307.5000000000000000, -56.99999999999997158, -169.9999999999999716 ) ) ;
#783 = ORIENTED_EDGE ( 'NONE', *, *, #12944, .F. ) ;
#784 = EDGE_LOOP ( 'NONE', ( #12621, #13135, #7197, #6469 ) ) ;
#785 = ADVANCED_FACE ( 'NONE', ( #6941 ), #9638, .T. ) ;
#786 = CARTESIAN_POINT ( 'NONE',  ( 0.000000000000000000, 0.5150000000000083400, -2.349999999999997424 ) ) ;
#787 = CIRCLE ( 'NONE', #4296, 2.649999999999985700 ) ;
#788 = AXIS2_PLACEMENT_3D ( 'NONE', #10096, #13425, #6557 ) ;
#789 = ORIENTED_EDGE ( 'NONE', *, *, #12859, .T. ) ;
#790 = PLANE ( 'NONE',  #910 ) ;
#791 = VERTEX_POINT ( 'NONE', #4709 ) ;
#792 = ORIENTED_EDGE ( 'NONE', *, *, #4975, .T. ) ;
#793 = CARTESIAN_POINT ( 'NONE',  ( -25.39999999999996305, 3.061616997868383141E-16, -2.500000000000000000 ) ) ;
#794 = VERTEX_POINT ( 'NONE', #5644 ) ;
#795 = LINE ( 'NONE', #13010, #2439 ) ;
#796 = UNCERTAINTY_MEASURE_WITH_UNIT (LENGTH_MEASURE( 1.000000000000000082E-05 ), #759, 'distance_accuracy_value', 'NONE');
#797 = CARTESIAN_POINT ( 'NONE',  ( 170.9999999999999716, -8.660254037844389075, 205.0000000000000284 ) ) ;
#798 = CARTESIAN_POINT ( 'NONE',  ( 319.9999999999999432, -20.00000000000000000, -169.9999999999999716 ) ) ;
#799 = ADVANCED_FACE ( 'NONE', ( #1417 ), #12246, .F. ) ;
#800 = EDGE_CURVE ( 'NONE', #11046, #2569, #4631, .T. ) ;
#801 = AXIS2_PLACEMENT_3D ( 'NONE', #6751, #6960, #5730 ) ;
#802 = EDGE_CURVE ( 'NONE', #6984, #1149, #10339, .T. ) ;
#803 = DIRECTION ( 'NONE',  ( -0.000000000000000000, 1.000000000000000000, 1.224646799147353207E-16 ) ) ;
#804 = FACE_OUTER_BOUND ( 'NONE', #5648, .T. ) ;
#805 = ORIENTED_EDGE ( 'NONE', *, *, #11640, .F. ) ;
#806 = VERTEX_POINT ( 'NONE', #6663 ) ;
#807 = DIRECTION ( 'NONE',  ( 0.000000000000000000, -1.000000000000000000, 0.000000000000000000 ) ) ;
#808 = CIRCLE ( 'NONE', #6622, 2.649999999999985700 ) ;
#809 = ORIENTED_EDGE ( 'NONE', *, *, #13309, .T. ) ;
#810 = DIRECTION ( 'NONE',  ( 1.000000000000000000, 0.000000000000000000, 0.000000000000000000 ) ) ;
#811 = CARTESIAN_POINT ( 'NONE',  ( 1.800000000000001155, 0.000000000000000000, 0.000000000000000000 ) ) ;
#812 = FACE_BOUND ( 'NONE', #4854, .T. ) ;
#813 = EDGE_LOOP ( 'NONE', ( #884, #4496, #11074, #5018, #198 ) ) ;
#814 = DIRECTION ( 'NONE',  ( 0.000000000000000000, -1.287488025362403787E-15, -1.000000000000000000 ) ) ;
#815 = AXIS2_PLACEMENT_3D ( 'NONE', #8559, #2026, #7322 ) ;
#816 = DIRECTION ( 'NONE',  ( 0.000000000000000000, 1.000000000000000000, 0.000000000000000000 ) ) ;
#817 = DIRECTION ( 'NONE',  ( 0.000000000000000000, 0.000000000000000000, 1.000000000000000000 ) ) ;
#818 = CARTESIAN_POINT ( 'NONE',  ( -5.000000000000000888, -8.660254037844389075, -210.0000000000000000 ) ) ;
#819 = CIRCLE ( 'NONE', #9878, 4.000000000000000000 ) ;
#820 = EDGE_LOOP ( 'NONE', ( #4312, #1747, #10761, #1441 ) ) ;
#821 =( REPRESENTATION_RELATIONSHIP ('NONE','NONE', #11251, #10314 ) REPRESENTATION_RELATIONSHIP_WITH_TRANSFORMATION ( #8837 )SHAPE_REPRESENTATION_RELATIONSHIP( ) );
#822 = EDGE_LOOP ( 'NONE', ( #3970, #8831, #13317, #6166 ) ) ;
#823 = CARTESIAN_POINT ( 'NONE',  ( 134.9999999999999432, -56.99999999999997158, -181.5021515430661054 ) ) ;
#824 = CIRCLE ( 'NONE', #346, 10.00000000000000000 ) ;
#825 = EDGE_CURVE ( 'NONE', #915, #3380, #3940, .T. ) ;
#826 = CARTESIAN_POINT ( 'NONE',  ( 302.6499999999999204, -95.00000000000008527, 186.2999999999999829 ) ) ;
#827 = CIRCLE ( 'NONE', #9659, 2.700000000000001066 ) ;
#828 = AXIS2_PLACEMENT_3D ( 'NONE', #1488, #13687, #385 ) ;
#829 = PRODUCT_DEFINITION_CONTEXT ( 'detailed design', #10547, 'design' ) ;
#830 = ORIENTED_EDGE ( 'NONE', *, *, #8702, .T. ) ;
#831 = DIRECTION ( 'NONE',  ( -0.000000000000000000, 1.000000000000000000, -0.000000000000000000 ) ) ;
#832 = CIRCLE ( 'NONE', #6862, 2.649999999999985700 ) ;
#833 = FACE_OUTER_BOUND ( 'NONE', #7177, .T. ) ;
#834 = CARTESIAN_POINT ( 'NONE',  ( 4.000000000000000000, 0.8378280264232961239, -3.220590601395640018 ) ) ;
#835 = CARTESIAN_POINT ( 'NONE',  ( 145.5000000000000284, -95.00000000000008527, -186.2999999999999829 ) ) ;
#836 = VECTOR ( 'NONE', #2195, 1000.000000000000000 ) ;
#837 = ORIENTED_EDGE ( 'NONE', *, *, #9419, .F. ) ;
#838 = AXIS2_PLACEMENT_3D ( 'NONE', #5898, #351, #4822 ) ;
#839 = PLANE ( 'NONE',  #11489 ) ;
#840 = VERTEX_POINT ( 'NONE', #10067 ) ;
#841 = EDGE_CURVE ( 'NONE', #7650, #1100, #97, .T. ) ;
#842 = CARTESIAN_POINT ( 'NONE',  ( 470.0000000000000000, -25.00000000000000000, 190.0000000000000000 ) ) ;
#843 = DIRECTION ( 'NONE',  ( 1.000000000000000000, 0.000000000000000000, 0.000000000000000000 ) ) ;
#844 = VECTOR ( 'NONE', #1170, 1000.000000000000000 ) ;
#845 = ORIENTED_EDGE ( 'NONE', *, *, #3733, .F. ) ;
#846 = FACE_OUTER_BOUND ( 'NONE', #14097, .T. ) ;
#847 = ORIENTED_EDGE ( 'NONE', *, *, #3069, .T. ) ;
#848 = CARTESIAN_POINT ( 'NONE',  ( 5.000000000000000888, 4.250000000000000000, 0.000000000000000000 ) ) ;
#849 = VECTOR ( 'NONE', #2245, 1000.000000000000000 ) ;
#850 = DIRECTION ( 'NONE',  ( 0.000000000000000000, 0.000000000000000000, 1.000000000000000000 ) ) ;
#851 = ORIENTED_EDGE ( 'NONE', *, *, #1764, .T. ) ;
#852 =( LENGTH_UNIT ( ) NAMED_UNIT ( * ) SI_UNIT ( .MILLI., .METRE. ) );
#853 = ADVANCED_FACE ( 'NONE', ( #8980 ), #9496, .T. ) ;
#854 = LINE ( 'NONE', #5313, #7831 ) ;
#855 = DIRECTION ( 'NONE',  ( 1.000000000000000000, 0.000000000000000000, 0.000000000000000000 ) ) ;
#856 = CARTESIAN_POINT ( 'NONE',  ( 197.5000000000000000, -90.00000000000007105, 55.00000000000001421 ) ) ;
#857 = ORIENTED_EDGE ( 'NONE', *, *, #8071, .F. ) ;
#858 = ORIENTED_EDGE ( 'NONE', *, *, #443, .F. ) ;
#859 = DIRECTION ( 'NONE',  ( -0.000000000000000000, -0.000000000000000000, -1.000000000000000000 ) ) ;
#860 = ORIENTED_EDGE ( 'NONE', *, *, #6657, .T. ) ;
#861 = CARTESIAN_POINT ( 'NONE',  ( 142.6500000000000057, -75.00000000000008527, 169.9999999999999716 ) ) ;
#862 = UNCERTAINTY_MEASURE_WITH_UNIT (LENGTH_MEASURE( 1.000000000000000082E-05 ), #515, 'distance_accuracy_value', 'NONE');
#863 = EDGE_LOOP ( 'NONE', ( #12473, #1825 ) ) ;
#864 = CONICAL_SURFACE ( 'NONE', #7822, 4.000000000000000000, 0.8911886515913786111 ) ;
#865 = VERTEX_POINT ( 'NONE', #13683 ) ;
#866 = CARTESIAN_POINT ( 'NONE',  ( -5.000000000000000888, -8.660254037844389075, -210.0000000000000000 ) ) ;
#867 = ORIENTED_EDGE ( 'NONE', *, *, #6061, .T. ) ;
#868 = LINE ( 'NONE', #3158, #1741 ) ;
#869 = LINE ( 'NONE', #935, #1336 ) ;
#870 = LINE ( 'NONE', #2049, #4107 ) ;
#871 = EDGE_CURVE ( 'NONE', #1382, #840, #5112, .T. ) ;
#872 = EDGE_CURVE ( 'NONE', #10300, #5386, #4179, .T. ) ;
#873 = PRESENTATION_STYLE_ASSIGNMENT (( #941 ) ) ;
#874 = DIRECTION ( 'NONE',  ( -1.000000000000000000, 0.000000000000000000, -0.000000000000000000 ) ) ;
#875 = ORIENTED_EDGE ( 'NONE', *, *, #339, .F. ) ;
#876 = AXIS2_PLACEMENT_3D ( 'NONE', #2252, #11112, #2107 ) ;
#877 = EDGE_LOOP ( 'NONE', ( #5483, #13862 ) ) ;
#878 = EDGE_CURVE ( 'NONE', #10453, #5579, #6146, .T. ) ;
#879 = CARTESIAN_POINT ( 'NONE',  ( 0.000000000000000000, 0.000000000000000000, 200.0000000000000000 ) ) ;
#880 = ORIENTED_EDGE ( 'NONE', *, *, #8701, .F. ) ;
#881 = CYLINDRICAL_SURFACE ( 'NONE', #3412, 2.649999999999985700 ) ;
#882 = CARTESIAN_POINT ( 'NONE',  ( -5.000000000000000888, 8.660254037844390851, 210.0000000000000000 ) ) ;
#883 = CARTESIAN_POINT ( 'NONE',  ( 0.3226060873438262311, -0.5149999999999915756, -2.189154565102686245 ) ) ;
#884 = ORIENTED_EDGE ( 'NONE', *, *, #7027, .T. ) ;
#885 = AXIS2_PLACEMENT_3D ( 'NONE', #13105, #14263, #2302 ) ;
#886 = ADVANCED_FACE ( 'NONE', ( #1485 ), #8095, .F. ) ;
#887 = CYLINDRICAL_SURFACE ( 'NONE', #1179, 5.500000000000005329 ) ;
#888 = CARTESIAN_POINT ( 'NONE',  ( -20.63749999999999929, 1.313433692085536673E-15, 10.72500000000000142 ) ) ;
#889 = DIRECTION ( 'NONE',  ( 6.123233995736766036E-17, 0.000000000000000000, 1.000000000000000000 ) ) ;
#890 = CARTESIAN_POINT ( 'NONE',  ( -4.024497503033714452, -2.323544716729502468, -3.572167766733752803 ) ) ;
#891 = ORIENTED_EDGE ( 'NONE', *, *, #9341, .F. ) ;
#892 = ORIENTED_EDGE ( 'NONE', *, *, #10216, .F. ) ;
#893 = AXIS2_PLACEMENT_3D ( 'NONE', #8075, #11492, #13514 ) ;
#894 = EDGE_CURVE ( 'NONE', #12837, #2710, #6725, .T. ) ;
#895 = PLANE ( 'NONE',  #11592 ) ;
#896 = EDGE_CURVE ( 'NONE', #1984, #11681, #9189, .T. ) ;
#897 = DIRECTION ( 'NONE',  ( -0.8571673013836870192, 1.049727191973306873E-16, 0.5150380737757234151 ) ) ;
#898 = VERTEX_POINT ( 'NONE', #607 ) ;
#899 = CYLINDRICAL_SURFACE ( 'NONE', #1302, 2.649999999999985700 ) ;
#900 = EDGE_CURVE ( 'NONE', #7113, #7167, #1368, .T. ) ;
#901 = CARTESIAN_POINT ( 'NONE',  ( 5.200000000000002842, 0.000000000000000000, 0.000000000000000000 ) ) ;
#902 = CARTESIAN_POINT ( 'NONE',  ( 30.00000000000002842, -225.0000000000000000, 339.9999999999999432 ) ) ;
#903 = CONTEXT_DEPENDENT_SHAPE_REPRESENTATION ( #13904, #11806 ) ;
#904 = ORIENTED_EDGE ( 'NONE', *, *, #1524, .T. ) ;
#905 = CARTESIAN_POINT ( 'NONE',  ( -0.7826237921249277196, 0.000000000000000000, 0.000000000000000000 ) ) ;
#906 = ORIENTED_EDGE ( 'NONE', *, *, #9206, .F. ) ;
#907 = CARTESIAN_POINT ( 'NONE',  ( 2.500000000000000000, 0.000000000000000000, 0.000000000000000000 ) ) ;
#908 = FACE_OUTER_BOUND ( 'NONE', #5250, .T. ) ;
#909 = AXIS2_PLACEMENT_3D ( 'NONE', #4923, #10280, #7233 ) ;
#910 = AXIS2_PLACEMENT_3D ( 'NONE', #6337, #9380, #9456 ) ;
#911 = ORIENTED_EDGE ( 'NONE', *, *, #13115, .T. ) ;
#912 = ORIENTED_EDGE ( 'NONE', *, *, #1614, .T. ) ;
#913 = FACE_OUTER_BOUND ( 'NONE', #14136, .T. ) ;
#914 = CARTESIAN_POINT ( 'NONE',  ( 2.740000000000000213, -0.5149999999999961275, -0.9838866223905694541 ) ) ;
#915 = VERTEX_POINT ( 'NONE', #10650 ) ;
#916 = FILL_AREA_STYLE_COLOUR ( '', #3433 ) ;
#917 = CIRCLE ( 'NONE', #12520, 2.649999999999985700 ) ;
#918 = PLANE ( 'NONE',  #2210 ) ;
#919 = ADVANCED_FACE ( 'NONE', ( #12596 ), #11585, .T. ) ;
#920 = FACE_OUTER_BOUND ( 'NONE', #822, .T. ) ;
#921 = CONTEXT_DEPENDENT_SHAPE_REPRESENTATION ( #4344, #1470 ) ;
#922 = CARTESIAN_POINT ( 'NONE',  ( -4.000000000000000000, 2.511478553582031203, -3.469254451724764543 ) ) ;
#923 = CIRCLE ( 'NONE', #1166, 13.29999999999999893 ) ;
#924 = VERTEX_POINT ( 'NONE', #12743 ) ;
#925 = EDGE_LOOP ( 'NONE', ( #10023, #943, #257, #1375 ) ) ;
#926 = CARTESIAN_POINT ( 'NONE',  ( 303.3333333333333144, -15.00000000000000000, 222.5000000000000853 ) ) ;
#927 = ORIENTED_EDGE ( 'NONE', *, *, #5351, .F. ) ;
#928 = CIRCLE ( 'NONE', #9057, 13.50000000000000000 ) ;
#929 = DIRECTION ( 'NONE',  ( -0.000000000000000000, -0.000000000000000000, 1.000000000000000000 ) ) ;
#930 = VERTEX_POINT ( 'NONE', #2815 ) ;
#931 = VERTEX_POINT ( 'NONE', #8233 ) ;
#932 = CARTESIAN_POINT ( 'NONE',  ( 206.0000000000000284, -85.00000000000007105, 190.0000000000000000 ) ) ;
#933 = ORIENTED_EDGE ( 'NONE', *, *, #11083, .T. ) ;
#934 = CARTESIAN_POINT ( 'NONE',  ( 2.740000000000000213, 0.9838866223909998876, -0.5150000000000000133 ) ) ;
#935 = CARTESIAN_POINT ( 'NONE',  ( -294.9999999999999432, -75.00000000000008527, 354.1421356237308942 ) ) ;
#936 = CIRCLE ( 'NONE', #6523, 2.649999999999985700 ) ;
#937 = B_SPLINE_CURVE_WITH_KNOTS ( 'NONE', 3,
 ( #2803, #953, #11940, #10924 ),
 .UNSPECIFIED., .F., .F.,
 ( 4, 4 ),
 ( 0.001586480565025038831, 0.004268227387428736967 ),
 .UNSPECIFIED. ) ;
#938 = CARTESIAN_POINT ( 'NONE',  ( 0.000000000000000000, -1.178949249685214307, 2.042000000000001592 ) ) ;
#939 = CARTESIAN_POINT ( 'NONE',  ( 5.000000000000002665, 3.306546357697854226E-16, 2.700000000000001066 ) ) ;
#940 = EDGE_CURVE ( 'NONE', #5316, #11325, #10663, .T. ) ;
#941 = SURFACE_STYLE_USAGE ( .BOTH. , #10702 ) ;
#942 = CARTESIAN_POINT ( 'NONE',  ( 303.3333333333333144, -20.00000000000000000, -222.5000000000000853 ) ) ;
#943 = ORIENTED_EDGE ( 'NONE', *, *, #2678, .T. ) ;
#944 = ORIENTED_EDGE ( 'NONE', *, *, #12577, .T. ) ;
#945 = VECTOR ( 'NONE', #1140, 1000.000000000000000 ) ;
#946 = CIRCLE ( 'NONE', #11369, 4.000000000000000000 ) ;
#947 = EDGE_CURVE ( 'NONE', #11046, #13697, #12507, .T. ) ;
#948 = DIRECTION ( 'NONE',  ( 0.000000000000000000, 0.000000000000000000, 1.000000000000000000 ) ) ;
#949 = AXIS2_PLACEMENT_3D ( 'NONE', #12351, #2413, #6766 ) ;
#950 = ADVANCED_FACE ( 'NONE', ( #2663 ), #533, .F. ) ;
#951 = ORIENTED_EDGE ( 'NONE', *, *, #6482, .F. ) ;
#952 = CARTESIAN_POINT ( 'NONE',  ( -2.100000000000000089, 2.571758278209441957E-16, -5.000000000000000000 ) ) ;
#953 = CARTESIAN_POINT ( 'NONE',  ( 0.9586399445693637444, -0.8293189044373081575, 0.5149999999999994582 ) ) ;
#954 = LINE ( 'NONE', #743, #10862 ) ;
#955 = ORIENTED_EDGE ( 'NONE', *, *, #10952, .T. ) ;
#956 = AXIS2_PLACEMENT_3D ( 'NONE', #8003, #1190, #5637 ) ;
#957 = CARTESIAN_POINT ( 'NONE',  ( 0.06760930072668894231, -0.9010842325122859764, 0.5149999999999992362 ) ) ;
#958 = CYLINDRICAL_SURFACE ( 'NONE', #7666, 2.649999999999985700 ) ;
#959 = LINE ( 'NONE', #7723, #4871 ) ;
#960 = CARTESIAN_POINT ( 'NONE',  ( 299.9999999999999432, -95.00000000000008527, 190.0000000000000000 ) ) ;
#961 = MECHANICAL_DESIGN_GEOMETRIC_PRESENTATION_REPRESENTATION (  '', ( #5399 ), #6555 ) ;
#962 = CARTESIAN_POINT ( 'NONE',  ( 82.99999999999998579, 8.660254037844390851, 205.0000000000000284 ) ) ;
#963 = AXIS2_PLACEMENT_3D ( 'NONE', #1507, #5945, #4658 ) ;
#964 = ORIENTED_EDGE ( 'NONE', *, *, #6331, .T. ) ;
#965 = ORIENTED_EDGE ( 'NONE', *, *, #7027, .F. ) ;
#966 = ADVANCED_FACE ( 'NONE', ( #8168 ), #7080, .T. ) ;
#967 = CARTESIAN_POINT ( 'NONE',  ( 386.6666666666666288, -25.00000000000000000, -225.1500000000000625 ) ) ;
#968 = EDGE_CURVE ( 'NONE', #546, #10685, #4921, .T. ) ;
#969 = VECTOR ( 'NONE', #7214, 1000.000000000000000 ) ;
#970 = DIRECTION ( 'NONE',  ( 0.000000000000000000, -1.000000000000000000, 0.000000000000000000 ) ) ;
#971 = AXIS2_PLACEMENT_3D ( 'NONE', #12444, #13808, #8300 ) ;
#972 = EDGE_CURVE ( 'NONE', #11786, #6378, #9409, .T. ) ;
#973 = ORIENTED_EDGE ( 'NONE', *, *, #5876, .T. ) ;
#974 = FACE_OUTER_BOUND ( 'NONE', #7536, .T. ) ;
#975 = CARTESIAN_POINT ( 'NONE',  ( 4.000000000000000000, -2.309401076758514915, -3.433295621305383349 ) ) ;
#976 = ADVANCED_FACE ( 'NONE', ( #12961, #7516, #14185, #4044 ), #6438, .F. ) ;
#977 = EDGE_CURVE ( 'NONE', #8679, #1004, #9030, .T. ) ;
#978 = DIRECTION ( 'NONE',  ( -0.000000000000000000, -0.000000000000000000, 1.000000000000000000 ) ) ;
#979 = DIRECTION ( 'NONE',  ( 0.000000000000000000, 0.000000000000000000, 1.000000000000000000 ) ) ;
#980 = EDGE_CURVE ( 'NONE', #3164, #7302, #13034, .T. ) ;
#981 = VERTEX_POINT ( 'NONE', #9708 ) ;
#982 = CARTESIAN_POINT ( 'NONE',  ( 119.9999999999999147, -225.0010000000000048, 169.9999999999999716 ) ) ;
#983 = PRODUCT_DEFINITION_SHAPE ( 'NONE', 'NONE',  #14312 ) ;
#984 = ORIENTED_EDGE ( 'NONE', *, *, #765, .F. ) ;
#985 = CARTESIAN_POINT ( 'NONE',  ( -0.1750025118121544265, -4.719839900820635314, -3.469254087858253399 ) ) ;
#986 = CARTESIAN_POINT ( 'NONE',  ( -299.9999999999999432, -75.00000000000008527, 11.50215154306610188 ) ) ;
#987 = ORIENTED_EDGE ( 'NONE', *, *, #3098, .F. ) ;
#988 = ORIENTED_EDGE ( 'NONE', *, *, #82, .T. ) ;
#989 = DIRECTION ( 'NONE',  ( -0.000000000000000000, -0.000000000000000000, 1.000000000000000000 ) ) ;
#990 = UNCERTAINTY_MEASURE_WITH_UNIT (LENGTH_MEASURE( 1.000000000000000082E-05 ), #187, 'distance_accuracy_value', 'NONE');
#991 = CARTESIAN_POINT ( 'NONE',  ( 305.0000000000000000, -56.99999999999997158, -180.0000000000000000 ) ) ;
#992 = B_SPLINE_CURVE_WITH_KNOTS ( 'NONE', 3,
 ( #9994, #2299, #1039, #13579, #10945, #11010 ),
 .UNSPECIFIED., .F., .F.,
 ( 4, 2, 4 ),
 ( 0.003358874760055551890, 0.004541967308452098118, 0.005725059856848645212 ),
 .UNSPECIFIED. ) ;
#993 = DIRECTION ( 'NONE',  ( -0.000000000000000000, 0.000000000000000000, 1.000000000000000000 ) ) ;
#994 = LINE ( 'NONE', #9059, #12994 ) ;
#995 = CARTESIAN_POINT ( 'NONE',  ( 132.4999999999999432, -56.99999999999997158, -169.9999999999999716 ) ) ;
#996 = DIRECTION ( 'NONE',  ( -1.000000000000000000, -2.775557561562893323E-15, 0.000000000000000000 ) ) ;
#997 = FILL_AREA_STYLE_COLOUR ( '', #8873 ) ;
#998 = DIRECTION ( 'NONE',  ( 1.000000000000000000, 0.000000000000000000, 0.000000000000000000 ) ) ;
#999 = CONTEXT_DEPENDENT_SHAPE_REPRESENTATION ( #8790, #13172 ) ;
#1000 = CARTESIAN_POINT ( 'NONE',  ( 307.5000000000000000, -36.99999999999997868, -180.0000000000000000 ) ) ;
#1001 = EDGE_LOOP ( 'NONE', ( #951, #1693, #8534, #1264, #9691, #5453, #13384, #1955 ) ) ;
#1002 = EDGE_LOOP ( 'NONE', ( #13804, #4995 ) ) ;
#1003 = FACE_OUTER_BOUND ( 'NONE', #2000, .T. ) ;
#1004 = VERTEX_POINT ( 'NONE', #11805 ) ;
#1005 = DIRECTION ( 'NONE',  ( -0.000000000000000000, -0.000000000000000000, -1.000000000000000000 ) ) ;
#1006 = VERTEX_POINT ( 'NONE', #967 ) ;
#1007 = EDGE_CURVE ( 'NONE', #8136, #2366, #3112, .T. ) ;
#1008 = VERTEX_POINT ( 'NONE', #12093 ) ;
#1009 = DIRECTION ( 'NONE',  ( -0.000000000000000000, -0.000000000000000000, 1.000000000000000000 ) ) ;
#1010 = EDGE_LOOP ( 'NONE', ( #11631, #9599, #14024, #3706 ) ) ;
#1011 = DIRECTION ( 'NONE',  ( -0.3090169943749412895, 1.164708318489094811E-16, -0.9510565162951555296 ) ) ;
#1012 = CARTESIAN_POINT ( 'NONE',  ( 136.6666666666666288, -20.00000000000000000, 222.5000000000000853 ) ) ;
#1013 = CARTESIAN_POINT ( 'NONE',  ( -30.00000000000002842, -25.00000000000000000, 169.9999999999999716 ) ) ;
#1014 = FACE_OUTER_BOUND ( 'NONE', #10764, .T. ) ;
#1015 =( REPRESENTATION_RELATIONSHIP ('NONE','NONE', #11251, #10796 ) REPRESENTATION_RELATIONSHIP_WITH_TRANSFORMATION ( #8549 )SHAPE_REPRESENTATION_RELATIONSHIP( ) );
#1016 = FILL_AREA_STYLE_COLOUR ( '', #1143 ) ;
#1017 = CARTESIAN_POINT ( 'NONE',  ( 2.500000000000000000, 1.178949249685213863, -2.042000000000001148 ) ) ;
#1018 = PRODUCT_DEFINITION_SHAPE ( 'NONE', 'NONE',  #14362 ) ;
#1019 = AXIS2_PLACEMENT_3D ( 'NONE', #11624, #9453, #1674 ) ;
#1020 = VERTEX_POINT ( 'NONE', #9776 ) ;
#1021 = ORIENTED_EDGE ( 'NONE', *, *, #11142, .T. ) ;
#1022 = FACE_OUTER_BOUND ( 'NONE', #3384, .T. ) ;
#1023 = EDGE_LOOP ( 'NONE', ( #4597, #2682 ) ) ;
#1024 = LINE ( 'NONE', #146, #12894 ) ;
#1025 = PLANE ( 'NONE',  #13721 ) ;
#1026 = CARTESIAN_POINT ( 'NONE',  ( 2.500000000000000000, 2.357898499370433054, -1.951563910473907981E-15 ) ) ;
#1027 = AXIS2_PLACEMENT_3D ( 'NONE', #5838, #6852, #3593 ) ;
#1028 = ORIENTED_EDGE ( 'NONE', *, *, #4301, .T. ) ;
#1029 = CARTESIAN_POINT ( 'NONE',  ( 8.000000000000000000, -4.896755294805453861E-15, 0.5150000000000000133 ) ) ;
#1030 = ADVANCED_FACE ( 'NONE', ( #753 ), #7415, .T. ) ;
#1031 = DIRECTION ( 'NONE',  ( -1.000000000000000000, -0.000000000000000000, -0.000000000000000000 ) ) ;
#1032 = CARTESIAN_POINT ( 'NONE',  ( 2.500000000000000000, -1.178949249685218303, -2.041999999999998039 ) ) ;
#1033 = ORIENTED_EDGE ( 'NONE', *, *, #13741, .F. ) ;
#1034 = CIRCLE ( 'NONE', #14250, 5.000000000000004441 ) ;
#1035 = AXIS2_PLACEMENT_3D ( 'NONE', #3051, #5502, #14059 ) ;
#1036 = CARTESIAN_POINT ( 'NONE',  ( 2.740000000000000213, -0.5150000000000034550, 0.9838866223909985553 ) ) ;
#1037 = CARTESIAN_POINT ( 'NONE',  ( 25.00000000000000000, 0.000000000000000000, 0.000000000000000000 ) ) ;
#1038 = EDGE_LOOP ( 'NONE', ( #284, #8064, #9090, #7106 ) ) ;
#1039 = CARTESIAN_POINT ( 'NONE',  ( 4.000000000000000000, -1.560351142792952617, -0.2242961665059816367 ) ) ;
#1040 = AXIS2_PLACEMENT_3D ( 'NONE', #7041, #3924, #2625 ) ;
#1041 = DIRECTION ( 'NONE',  ( -0.000000000000000000, 1.000000000000000000, 0.000000000000000000 ) ) ;
#1042 = ADVANCED_FACE ( 'NONE', ( #6284 ), #8457, .F. ) ;
#1043 = CIRCLE ( 'NONE', #374, 5.000000000000004441 ) ;
#1044 = CARTESIAN_POINT ( 'NONE',  ( 124.9999999999999858, 55.00000000000000711, 10.00000000000000000 ) ) ;
#1045 = CARTESIAN_POINT ( 'NONE',  ( 386.6666666666666288, -10.00000000000000000, 222.5000000000000853 ) ) ;
#1046 = CONTEXT_DEPENDENT_SHAPE_REPRESENTATION ( #1565, #8315 ) ;
#1047 = AXIS2_PLACEMENT_3D ( 'NONE', #6540, #14218, #10826 ) ;
#1048 = ORIENTED_EDGE ( 'NONE', *, *, #6214, .T. ) ;
#1049 = TOROIDAL_SURFACE ( 'NONE', #4558, 10.20000000000000107, 0.2000000000000031197 ) ;
#1050 = CYLINDRICAL_SURFACE ( 'NONE', #1035, 2.649999999999985700 ) ;
#1051 = VERTEX_POINT ( 'NONE', #5213 ) ;
#1052 = DIRECTION ( 'NONE',  ( -1.000000000000000000, 0.000000000000000000, 0.000000000000000000 ) ) ;
#1053 = DIRECTION ( 'NONE',  ( -0.000000000000000000, 0.000000000000000000, -1.000000000000000000 ) ) ;
#1054 = ADVANCED_BREP_SHAPE_REPRESENTATION ( '', ( #8362, #14039 ), #4925 ) ;
#1055 = ADVANCED_FACE ( 'NONE', ( #8538 ), #2001, .T. ) ;
#1056 = EDGE_CURVE ( 'NONE', #13697, #10145, #8756, .T. ) ;
#1057 = VECTOR ( 'NONE', #6494, 1000.000000000000000 ) ;
#1058 = ORIENTED_EDGE ( 'NONE', *, *, #8177, .F. ) ;
#1059 = ORIENTED_EDGE ( 'NONE', *, *, #4977, .F. ) ;
#1060 = DIRECTION ( 'NONE',  ( 0.000000000000000000, -1.000000000000000000, 0.000000000000000000 ) ) ;
#1061 = DIRECTION ( 'NONE',  ( 0.000000000000000000, 0.5000000000000012212, 0.8660254037844380415 ) ) ;
#1062 = AXIS2_PLACEMENT_3D ( 'NONE', #12681, #2536, #5795 ) ;
#1063 = DIRECTION ( 'NONE',  ( 0.000000000000000000, 0.000000000000000000, -1.000000000000000000 ) ) ;
#1064 = EDGE_CURVE ( 'NONE', #10103, #13709, #11359, .T. ) ;
#1065 = DIRECTION ( 'NONE',  ( -0.000000000000000000, -1.000000000000000000, -0.000000000000000000 ) ) ;
#1066 = AXIS2_PLACEMENT_3D ( 'NONE', #12203, #2342, #2270 ) ;
#1067 = LINE ( 'NONE', #11036, #3067 ) ;
#1068 = CYLINDRICAL_SURFACE ( 'NONE', #8248, 5.500000000000005329 ) ;
#1069 = FACE_OUTER_BOUND ( 'NONE', #2025, .T. ) ;
#1070 = VECTOR ( 'NONE', #2045, 1000.000000000000000 ) ;
#1071 = CARTESIAN_POINT ( 'NONE',  ( -1.317756351988340180, 3.857995168970202116, -0.04852650426601388955 ) ) ;
#1072 = ORIENTED_EDGE ( 'NONE', *, *, #85, .F. ) ;
#1073 = EDGE_LOOP ( 'NONE', ( #667, #1257, #1363 ) ) ;
#1074 = LINE ( 'NONE', #5527, #776 ) ;
#1075 = AXIS2_PLACEMENT_3D ( 'NONE', #7410, #2850, #7263 ) ;
#1076 = ORIENTED_EDGE ( 'NONE', *, *, #6538, .F. ) ;
#1077 = CARTESIAN_POINT ( 'NONE',  ( 229.9999999999999432, -85.00000000000007105, 170.0000000000000000 ) ) ;
#1078 = ADVANCED_FACE ( 'NONE', ( #3255 ), #895, .T. ) ;
#1079 = CIRCLE ( 'NONE', #5291, 2.500000000000000888 ) ;
#1080 = EDGE_CURVE ( 'NONE', #14253, #2215, #14042, .T. ) ;
#1081 = ORIENTED_EDGE ( 'NONE', *, *, #2069, .F. ) ;
#1082 = DIRECTION ( 'NONE',  ( 1.000000000000000000, 0.000000000000000000, 0.000000000000000000 ) ) ;
#1083 = ORIENTED_EDGE ( 'NONE', *, *, #13637, .F. ) ;
#1084 = DIRECTION ( 'NONE',  ( -0.000000000000000000, -0.000000000000000000, 1.000000000000000000 ) ) ;
#1085 = CONICAL_SURFACE ( 'NONE', #9208, 4.000000000000000000, 0.8911886515913786111 ) ;
#1086 = CIRCLE ( 'NONE', #12451, 2.500000000000002220 ) ;
#1087 = DIRECTION ( 'NONE',  ( 0.000000000000000000, 1.000000000000000000, 0.000000000000000000 ) ) ;
#1088 = CARTESIAN_POINT ( 'NONE',  ( 2.500000000000000000, 1.178949249685218525, 2.041999999999999371 ) ) ;
#1089 = EDGE_CURVE ( 'NONE', #12823, #2998, #6949, .T. ) ;
#1090 = CARTESIAN_POINT ( 'NONE',  ( -140.0000000000000000, -95.00000000000008527, 40.00000000000000000 ) ) ;
#1091 =( LENGTH_UNIT ( ) NAMED_UNIT ( * ) SI_UNIT ( .MILLI., .METRE. ) );
#1092 = SURFACE_SIDE_STYLE ('',( #10171 ) ) ;
#1093 = B_SPLINE_CURVE_WITH_KNOTS ( 'NONE', 3,
 ( #5901, #4967, #2642, #286 ),
 .UNSPECIFIED., .F., .F.,
 ( 4, 4 ),
 ( 0.001586480563516616538, 0.004268227385920363680 ),
 .UNSPECIFIED. ) ;
#1094 = AXIS2_PLACEMENT_3D ( 'NONE', #7522, #1790, #13978 ) ;
#1095 = DIRECTION ( 'NONE',  ( 0.000000000000000000, 0.000000000000000000, -1.000000000000000000 ) ) ;
#1096 = ORIENTED_EDGE ( 'NONE', *, *, #3247, .F. ) ;
#1097 = AXIS2_PLACEMENT_3D ( 'NONE', #1465, #6917, #7059 ) ;
#1098 = VERTEX_POINT ( 'NONE', #6363 ) ;
#1099 = CARTESIAN_POINT ( 'NONE',  ( -2.000000000000001776, 1.641026710857453312E-15, 13.29999999999999893 ) ) ;
#1100 = VERTEX_POINT ( 'NONE', #679 ) ;
#1101 = CYLINDRICAL_SURFACE ( 'NONE', #5026, 2.649999999999985700 ) ;
#1102 = CARTESIAN_POINT ( 'NONE',  ( 2.740000000000000213, 0.5150000000000035660, -0.9838866223905657904 ) ) ;
#1103 = VERTEX_POINT ( 'NONE', #7658 ) ;
#1104 = DIRECTION ( 'NONE',  ( -1.000000000000000000, -0.000000000000000000, -0.000000000000000000 ) ) ;
#1105 = AXIS2_PLACEMENT_3D ( 'NONE', #1329, #11353, #13588 ) ;
#1106 = PLANE ( 'NONE',  #10917 ) ;
#1107 = LINE ( 'NONE', #5555, #2077 ) ;
#1108 = PRODUCT_DEFINITION_SHAPE ( 'NONE', 'NONE',  #14320 ) ;
#1109 = DIRECTION ( 'NONE',  ( -0.000000000000000000, 1.000000000000000000, -0.000000000000000000 ) ) ;
#1110 = EDGE_CURVE ( 'NONE', #8867, #8759, #4189, .T. ) ;
#1111 = VERTEX_POINT ( 'NONE', #9561 ) ;
#1112 = AXIS2_PLACEMENT_3D ( 'NONE', #2555, #4882, #5958 ) ;
#1113 = PLANE ( 'NONE',  #4657 ) ;
#1114 = FACE_OUTER_BOUND ( 'NONE', #12708, .T. ) ;
#1115 = AXIS2_PLACEMENT_3D ( 'NONE', #7614, #13204, #12122 ) ;
#1116 = DIRECTION ( 'NONE',  ( 0.000000000000000000, 1.000000000000000000, 0.000000000000000000 ) ) ;
#1117 = ORIENTED_EDGE ( 'NONE', *, *, #9700, .F. ) ;
#1118 = LINE ( 'NONE', #2643, #11978 ) ;
#1119 = CARTESIAN_POINT ( 'NONE',  ( 0.000000000000000000, 5.051668046482832750E-16, -4.000000000000000000 ) ) ;
#1120 = DIRECTION ( 'NONE',  ( -0.000000000000000000, -0.000000000000000000, -1.000000000000000000 ) ) ;
#1121 = CARTESIAN_POINT ( 'NONE',  ( 0.000000000000000000, 0.000000000000000000, 0.000000000000000000 ) ) ;
#1122 = VECTOR ( 'NONE', #11092, 1000.000000000000000 ) ;
#1123 = CONTEXT_DEPENDENT_SHAPE_REPRESENTATION ( #1765, #534 ) ;
#1124 = AXIS2_PLACEMENT_3D ( 'NONE', #13971, #12956, #3031 ) ;
#1125 = VERTEX_POINT ( 'NONE', #823 ) ;
#1126 = LINE ( 'NONE', #3408, #12403 ) ;
#1127 = VERTEX_POINT ( 'NONE', #2492 ) ;
#1128 = DIRECTION ( 'NONE',  ( 0.000000000000000000, 0.000000000000000000, 1.000000000000000000 ) ) ;
#1129 = EDGE_CURVE ( 'NONE', #4266, #2405, #348, .T. ) ;
#1130 = ADVANCED_FACE ( 'NONE', ( #2636, #11413 ), #1113, .F. ) ;
#1131 = ORIENTED_EDGE ( 'NONE', *, *, #12517, .F. ) ;
#1132 = ORIENTED_EDGE ( 'NONE', *, *, #2253, .T. ) ;
#1133 = CIRCLE ( 'NONE', #9492, 2.500000000000002220 ) ;
#1134 = DIRECTION ( 'NONE',  ( -1.000000000000000000, 0.000000000000000000, 0.000000000000000000 ) ) ;
#1135 = DIRECTION ( 'NONE',  ( 1.000000000000000000, 0.000000000000000000, 0.000000000000000000 ) ) ;
#1136 = AXIS2_PLACEMENT_3D ( 'NONE', #13097, #6510, #14116 ) ;
#1137 = DIRECTION ( 'NONE',  ( 0.000000000000000000, -1.000000000000000000, 0.000000000000000000 ) ) ;
#1138 = AXIS2_PLACEMENT_3D ( 'NONE', #13702, #10598, #12689 ) ;
#1139 = LINE ( 'NONE', #5516, #526 ) ;
#1140 = DIRECTION ( 'NONE',  ( -0.000000000000000000, 1.000000000000000000, -0.000000000000000000 ) ) ;
#1141 = DIRECTION ( 'NONE',  ( -0.000000000000000000, -0.000000000000000000, 1.000000000000000000 ) ) ;
#1142 = SURFACE_STYLE_FILL_AREA ( #2394 ) ;
#1143 = COLOUR_RGB ( '',0.8941176470588234615, 0.8941176470588234615, 0.8941176470588234615 ) ;
#1144 = CARTESIAN_POINT ( 'NONE',  ( 2.500000000000000000, -2.629050547790028551E-15, -2.041999999999999815 ) ) ;
#1145 = CONTEXT_DEPENDENT_SHAPE_REPRESENTATION ( #6038, #13289 ) ;
#1146 = EDGE_CURVE ( 'NONE', #10315, #11952, #6039, .T. ) ;
#1147 = CARTESIAN_POINT ( 'NONE',  ( 0.000000000000000000, 0.5149999999999917977, 2.350000000000000089 ) ) ;
#1148 = EDGE_LOOP ( 'NONE', ( #13554, #3782, #7353, #9523 ) ) ;
#1149 = VERTEX_POINT ( 'NONE', #11481 ) ;
#1150 = CARTESIAN_POINT ( 'NONE',  ( 1.849560077140141257, 0.7556913915602415655, -0.5150000000000000133 ) ) ;
#1151 = VERTEX_POINT ( 'NONE', #8203 ) ;
#1152 = VECTOR ( 'NONE', #8133, 1000.000000000000000 ) ;
#1153 = CARTESIAN_POINT ( 'NONE',  ( 2.500000000000000000, -1.178949249685213863, 2.042000000000002924 ) ) ;
#1154 = EDGE_CURVE ( 'NONE', #3317, #2814, #8816, .T. ) ;
#1155 = EDGE_CURVE ( 'NONE', #12855, #4614, #1461, .T. ) ;
#1156 = EDGE_LOOP ( 'NONE', ( #5436, #9530, #5592, #6967 ) ) ;
#1157 = DIRECTION ( 'NONE',  ( -0.000000000000000000, -0.000000000000000000, -1.000000000000000000 ) ) ;
#1158 = EDGE_LOOP ( 'NONE', ( #6888, #7499, #114, #558 ) ) ;
#1159 = VECTOR ( 'NONE', #2534, 1000.000000000000000 ) ;
#1160 = CYLINDRICAL_SURFACE ( 'NONE', #8697, 5.000000000000004441 ) ;
#1161 = CARTESIAN_POINT ( 'NONE',  ( 3.999999999999999112, 2.309401076758497595, -3.504271511727124366 ) ) ;
#1162 = EDGE_CURVE ( 'NONE', #1127, #2687, #4887, .T. ) ;
#1163 = DIRECTION ( 'NONE',  ( 1.007709689656716938E-16, 1.000000000000000000, 3.606821995490528048E-15 ) ) ;
#1164 = CARTESIAN_POINT ( 'NONE',  ( 140.0000000000000000, -75.00000000000008527, 186.2999999999999829 ) ) ;
#1165 = SURFACE_STYLE_FILL_AREA ( #130 ) ;
#1166 = AXIS2_PLACEMENT_3D ( 'NONE', #9397, #12514, #7069 ) ;
#1167 = CARTESIAN_POINT ( 'NONE',  ( -314.9999999999999432, 55.00000000000001421, 30.00000000000000000 ) ) ;
#1168 = ADVANCED_FACE ( 'NONE', ( #13249 ), #9988, .F. ) ;
#1169 = EDGE_CURVE ( 'NONE', #1125, #9107, #13723, .T. ) ;
#1170 = DIRECTION ( 'NONE',  ( -0.000000000000000000, 1.000000000000000000, 0.000000000000000000 ) ) ;
#1171 =( REPRESENTATION_RELATIONSHIP ('NONE','NONE', #11251, #3832 ) REPRESENTATION_RELATIONSHIP_WITH_TRANSFORMATION ( #6393 )SHAPE_REPRESENTATION_RELATIONSHIP( ) );
#1172 = EDGE_LOOP ( 'NONE', ( #1315, #8576 ) ) ;
#1173 = ADVANCED_FACE ( 'NONE', ( #9235, #6910 ), #3583, .F. ) ;
#1174 = ADVANCED_FACE ( 'NONE', ( #7983 ), #4410, .T. ) ;
#1175 = VECTOR ( 'NONE', #5759, 1000.000000000000000 ) ;
#1176 = ORIENTED_EDGE ( 'NONE', *, *, #293, .F. ) ;
#1177 = EDGE_CURVE ( 'NONE', #7747, #14235, #6647, .T. ) ;
#1178 = DIRECTION ( 'NONE',  ( 1.000000000000000000, 0.000000000000000000, 0.000000000000000000 ) ) ;
#1179 = AXIS2_PLACEMENT_3D ( 'NONE', #10929, #10718, #7581 ) ;
#1180 = ORIENTED_EDGE ( 'NONE', *, *, #12121, .F. ) ;
#1181 = DIRECTION ( 'NONE',  ( -0.000000000000000000, 0.000000000000000000, 1.000000000000000000 ) ) ;
#1182 = CARTESIAN_POINT ( 'NONE',  ( 136.6666666666666288, -20.00000000000000000, 222.5000000000000853 ) ) ;
#1183 = CARTESIAN_POINT ( 'NONE',  ( 294.4999999999999432, -75.00000000000008527, -190.0000000000000000 ) ) ;
#1184 = DIRECTION ( 'NONE',  ( 0.000000000000000000, 1.000000000000000000, 1.086455722314322026E-16 ) ) ;
#1185 = LINE ( 'NONE', #5687, #3265 ) ;
#1186 = DIRECTION ( 'NONE',  ( -0.000000000000000000, 1.000000000000000000, -0.000000000000000000 ) ) ;
#1187 = CARTESIAN_POINT ( 'NONE',  ( 299.9999999999999432, -75.00000000000008527, -186.2999999999999829 ) ) ;
#1188 = VERTEX_POINT ( 'NONE', #3330 ) ;
#1189 = LINE ( 'NONE', #5768, #6517 ) ;
#1190 = DIRECTION ( 'NONE',  ( 1.000000000000000000, 0.000000000000000000, 0.000000000000000000 ) ) ;
#1191 = VECTOR ( 'NONE', #7717, 1000.000000000000000 ) ;
#1192 = CARTESIAN_POINT ( 'NONE',  ( 470.0000000000000000, -25.00000000000000000, 250.0000000000000000 ) ) ;
#1193 = ADVANCED_FACE ( 'NONE', ( #9918 ), #9336, .F. ) ;
#1194 = ORIENTED_EDGE ( 'NONE', *, *, #2773, .T. ) ;
#1195 = CARTESIAN_POINT ( 'NONE',  ( 305.4999999999999432, -95.00000000000008527, 186.2999999999999829 ) ) ;
#1196 = AXIS2_PLACEMENT_3D ( 'NONE', #7294, #11799, #1705 ) ;
#1197 = PLANE ( 'NONE',  #14279 ) ;
#1198 = AXIS2_PLACEMENT_3D ( 'NONE', #10088, #4870, #4583 ) ;
#1199 = FACE_OUTER_BOUND ( 'NONE', #9157, .T. ) ;
#1200 = DIRECTION ( 'NONE',  ( 0.000000000000000000, 0.000000000000000000, -1.000000000000000000 ) ) ;
#1202 = AXIS2_PLACEMENT_3D ( 'NONE', #11836, #12995, #2993 ) ;
#1201 = VECTOR ( 'NONE', #13083, 1000.000000000000000 ) ;
#1203 = ORIENTED_EDGE ( 'NONE', *, *, #5421, .T. ) ;
#1204 = LINE ( 'NONE', #12460, #4769 ) ;
#1205 =( NAMED_UNIT ( * ) SI_UNIT ( $, .STERADIAN. ) SOLID_ANGLE_UNIT ( ) );
#1206 =( GEOMETRIC_REPRESENTATION_CONTEXT ( 3 ) GLOBAL_UNCERTAINTY_ASSIGNED_CONTEXT ( ( #1912 ) ) GLOBAL_UNIT_ASSIGNED_CONTEXT ( ( #12564, #13563, #1591 ) ) REPRESENTATION_CONTEXT ( 'NONE', 'WORKASPACE' ) );
#1207 = ORIENTED_EDGE ( 'NONE', *, *, #11435, .T. ) ;
#1208 = CARTESIAN_POINT ( 'NONE',  ( 0.000000000000000000, -1.178949249685213863, 2.042000000000002924 ) ) ;
#1209 = ORIENTED_EDGE ( 'NONE', *, *, #1854, .T. ) ;
#1210 = ORIENTED_EDGE ( 'NONE', *, *, #9443, .F. ) ;
#1211 = LINE ( 'NONE', #7951, #14259 ) ;
#1212 = DIRECTION ( 'NONE',  ( -1.000000000000000000, 0.000000000000000000, 0.000000000000000000 ) ) ;
#1213 = AXIS2_PLACEMENT_3D ( 'NONE', #3991, #6162, #7918 ) ;
#1214 = DIRECTION ( 'NONE',  ( 0.000000000000000000, -0.000000000000000000, 1.000000000000000000 ) ) ;
#1215 = DIRECTION ( 'NONE',  ( -0.000000000000000000, -0.000000000000000000, 1.000000000000000000 ) ) ;
#1216 = DIRECTION ( 'NONE',  ( -0.000000000000000000, -0.000000000000000000, 1.000000000000000000 ) ) ;
#1217 = DIRECTION ( 'NONE',  ( 2.775557561562893323E-15, -1.000000000000000000, 0.000000000000000000 ) ) ;
#1218 = SHAPE_REPRESENTATION_RELATIONSHIP ( 'NONE' , 'NONE' ,  #7730, #6958 ) ;
#1219 = B_SPLINE_CURVE_WITH_KNOTS ( 'NONE', 3,
 ( #7556, #4084, #14301, #9750 ),
 .UNSPECIFIED., .F., .F.,
 ( 4, 4 ),
 ( 0.004656695504653254707, 0.007337072591785142629 ),
 .UNSPECIFIED. ) ;
#1220 = DIRECTION ( 'NONE',  ( 0.000000000000000000, 0.000000000000000000, -1.000000000000000000 ) ) ;
#1221 = EDGE_CURVE ( 'NONE', #8720, #14065, #6982, .T. ) ;
#1222 = CONTEXT_DEPENDENT_SHAPE_REPRESENTATION ( #8535, #3133 ) ;
#1223 = ORIENTED_EDGE ( 'NONE', *, *, #9152, .T. ) ;
#1224 = ORIENTED_EDGE ( 'NONE', *, *, #3247, .T. ) ;
#1225 = CARTESIAN_POINT ( 'NONE',  ( 0.000000000000000000, 0.5149999999999917977, 2.350000000000000089 ) ) ;
#1226 = ORIENTED_EDGE ( 'NONE', *, *, #3673, .F. ) ;
#1227 = LINE ( 'NONE', #3497, #6780 ) ;
#1228 = ORIENTED_EDGE ( 'NONE', *, *, #5685, .F. ) ;
#1229 = DIRECTION ( 'NONE',  ( -1.000000000000000000, -0.000000000000000000, -0.000000000000000000 ) ) ;
#1230 = ORIENTED_EDGE ( 'NONE', *, *, #4069, .T. ) ;
#1231 = PLANE ( 'NONE',  #3603 ) ;
#1232 = PRODUCT_DEFINITION_SHAPE ( 'NONE', 'NONE',  #6314 ) ;
#1233 = DIRECTION ( 'NONE',  ( 0.000000000000000000, 0.000000000000000000, 1.000000000000000000 ) ) ;
#1234 =( LENGTH_UNIT ( ) NAMED_UNIT ( * ) SI_UNIT ( .MILLI., .METRE. ) );
#1235 = PLANE ( 'NONE',  #9389 ) ;
#1236 =( NAMED_UNIT ( * ) SI_UNIT ( $, .STERADIAN. ) SOLID_ANGLE_UNIT ( ) );
#1237 = ADVANCED_FACE ( 'NONE', ( #12422 ), #3096, .F. ) ;
#1238 = CARTESIAN_POINT ( 'NONE',  ( 140.0000000000000000, -75.00000000000008527, 190.0000000000000000 ) ) ;
#1239 = PRODUCT_RELATED_PRODUCT_CATEGORY ( 'part', '', ( #6922 ) ) ;
#1240 = DIRECTION ( 'NONE',  ( 0.000000000000000000, 0.000000000000000000, 1.000000000000000000 ) ) ;
#1241 =( BOUNDED_SURFACE ( )  B_SPLINE_SURFACE ( 3, 2, ( 
 ( #1646, #10588, #6229 ),
 ( #1799, #6156, #3983 ),
 ( #9575, #11745, #7310 ),
 ( #13981, #11672, #6086 ),
 ( #2751, #10514, #12754 ),
 ( #8399, #12828, #9425 ) ),
 .UNSPECIFIED., .F., .F., .F. ) 
 B_SPLINE_SURFACE_WITH_KNOTS ( ( 4, 2, 4 ),
 ( 3, 3 ),
 ( 0.02032853247518125531, 0.02278863295364820865, 0.02524873343211516200 ),
 ( 0.000000000000000000, 1.000000000000000000 ),
 .UNSPECIFIED. ) 
 GEOMETRIC_REPRESENTATION_ITEM ( )  RATIONAL_B_SPLINE_SURFACE ( (
 ( 1.000000000000000000, 0.8047781615896836271, 1.000000000000000000),
 ( 1.000000000000000000, 0.8123767586289967202, 1.000000000000000000),
 ( 1.000000000000000000, 0.8190662415563443322, 1.000000000000000000),
 ( 1.000000000000000000, 0.8192361015669982205, 1.000000000000000000),
 ( 1.000000000000000000, 0.8126135807103181952, 1.000000000000000000),
 ( 1.000000000000000000, 0.8047712338318587788, 1.000000000000000000) ) ) 
 REPRESENTATION_ITEM ( '' )  SURFACE ( )  );
#1242 = ORIENTED_EDGE ( 'NONE', *, *, #13470, .F. ) ;
#1243 = VERTEX_POINT ( 'NONE', #9159 ) ;
#1244 = VERTEX_POINT ( 'NONE', #10316 ) ;
#1245 = CARTESIAN_POINT ( 'NONE',  ( 233.8499999999999375, -85.00000000000007105, 55.00000000000001421 ) ) ;
#1246 = ORIENTED_EDGE ( 'NONE', *, *, #7530, .T. ) ;
#1247 = CARTESIAN_POINT ( 'NONE',  ( -124.9999999999999432, -105.0000000000000853, 40.00000000000000000 ) ) ;
#1248 = ADVANCED_BREP_SHAPE_REPRESENTATION ( '', ( #3687, #14039 ), #1895 ) ;
#1249 = CARTESIAN_POINT ( 'NONE',  ( -31.74999999999995737, 0.000000000000000000, 0.000000000000000000 ) ) ;
#1250 = EDGE_CURVE ( 'NONE', #4587, #12687, #13572, .T. ) ;
#1251 = ADVANCED_FACE ( 'NONE', ( #14005, #5249 ), #790, .F. ) ;
#1252 = EDGE_CURVE ( 'NONE', #3125, #6716, #11626, .T. ) ;
#1253 = CARTESIAN_POINT ( 'NONE',  ( -297.4999999999999432, -75.00000000000008527, 339.9999999999999432 ) ) ;
#1254 = CARTESIAN_POINT ( 'NONE',  ( 4.000000000000000000, 1.680228229147133767, -3.316631783032546021 ) ) ;
#1255 = CARTESIAN_POINT ( 'NONE',  ( 0.06760930072668842883, -0.5149999999999961275, -0.9010842325122929708 ) ) ;
#1256 = DIRECTION ( 'NONE',  ( 0.000000000000000000, 0.000000000000000000, -1.000000000000000000 ) ) ;
#1257 = ORIENTED_EDGE ( 'NONE', *, *, #1636, .T. ) ;
#1258 = CIRCLE ( 'NONE', #12860, 2.500000000000001332 ) ;
#1259 = AXIS2_PLACEMENT_3D ( 'NONE', #225, #6483, #4453 ) ;
#1260 = CARTESIAN_POINT ( 'NONE',  ( 136.6666666666666288, -25.00000000000000000, 222.5000000000000853 ) ) ;
#1261 = CARTESIAN_POINT ( 'NONE',  ( -2.345747346278108214, 3.264484291692489215, -0.01223254789873409049 ) ) ;
#1262 = EDGE_CURVE ( 'NONE', #12287, #4042, #3951, .T. ) ;
#1263 = DIRECTION ( 'NONE',  ( -1.000000000000000000, -0.000000000000000000, -0.000000000000000000 ) ) ;
#1264 = ORIENTED_EDGE ( 'NONE', *, *, #4414, .T. ) ;
#1265 = FACE_BOUND ( 'NONE', #12172, .T. ) ;
#1266 = DIRECTION ( 'NONE',  ( -1.000000000000000000, 0.000000000000000000, 0.000000000000000000 ) ) ;
#1267 = DIRECTION ( 'NONE',  ( 6.123233995736766036E-17, -1.000000000000000000, 0.000000000000000000 ) ) ;
#1268 = B_SPLINE_CURVE_WITH_KNOTS ( 'NONE', 3,
 ( #2988, #4066, #5310, #557, #14135, #9731, #10817, #13854 ),
 .UNSPECIFIED., .F., .F.,
 ( 4, 2, 2, 4 ),
 ( 0.005725059856848641743, 0.006314084072593626612, 0.006903108288338611481, 0.008081156719828581220 ),
 .UNSPECIFIED. ) ;
#1269 = CONTEXT_DEPENDENT_SHAPE_REPRESENTATION ( #4008, #662 ) ;
#1270 = ORIENTED_EDGE ( 'NONE', *, *, #7944, .T. ) ;
#1271 = DIRECTION ( 'NONE',  ( 0.000000000000000000, 1.000000000000000000, 0.000000000000000000 ) ) ;
#1272 = EDGE_LOOP ( 'NONE', ( #1972, #8916, #242, #11309, #9922 ) ) ;
#1273 = CARTESIAN_POINT ( 'NONE',  ( -13.50000000000000000, 1.653273178848926867E-15, 186.0000000000000000 ) ) ;
#1274 = CIRCLE ( 'NONE', #7988, 5.384454397937118664 ) ;
#1275 = VERTEX_POINT ( 'NONE', #12852 ) ;
#1276 = ORIENTED_EDGE ( 'NONE', *, *, #9037, .T. ) ;
#1277 = DIRECTION ( 'NONE',  ( 0.000000000000000000, -1.000000000000000000, 0.000000000000000000 ) ) ;
#1278 = FACE_OUTER_BOUND ( 'NONE', #13437, .T. ) ;
#1279 = DIRECTION ( 'NONE',  ( -0.000000000000000000, -0.000000000000000000, 1.000000000000000000 ) ) ;
#1280 = CARTESIAN_POINT ( 'NONE',  ( 210.0000000000000000, -85.00000000000007105, 55.00000000000002132 ) ) ;
#1281 = LINE ( 'NONE', #5721, #945 ) ;
#1282 = DIRECTION ( 'NONE',  ( -0.000000000000000000, -0.000000000000000000, 1.000000000000000000 ) ) ;
#1283 = AXIS2_PLACEMENT_3D ( 'NONE', #3071, #1894, #4292 ) ;
#1284 = DIRECTION ( 'NONE',  ( -0.000000000000000000, -0.000000000000000000, -1.000000000000000000 ) ) ;
#1285 = ITEM_DEFINED_TRANSFORMATION ( 'NONE', 'NONE', #2373,  #14039 ) ;
#1286 = AXIS2_PLACEMENT_3D ( 'NONE', #9219, #6100, #8120 ) ;
#1287 = ORIENTED_EDGE ( 'NONE', *, *, #13354, .T. ) ;
#1288 = EDGE_CURVE ( 'NONE', #1020, #2372, #9042, .T. ) ;
#1289 = ORIENTED_EDGE ( 'NONE', *, *, #7359, .T. ) ;
#1290 = AXIS2_PLACEMENT_3D ( 'NONE', #7574, #8668, #14169 ) ;
#1291 = CARTESIAN_POINT ( 'NONE',  ( 470.0000000000000000, -20.00000000000000000, 250.0000000000000000 ) ) ;
#1292 =( REPRESENTATION_RELATIONSHIP ('NONE','NONE', #11251, #208 ) REPRESENTATION_RELATIONSHIP_WITH_TRANSFORMATION ( #9592 )SHAPE_REPRESENTATION_RELATIONSHIP( ) );
#1293 = ORIENTED_EDGE ( 'NONE', *, *, #9936, .T. ) ;
#1294 = CARTESIAN_POINT ( 'NONE',  ( -299.9999999999999432, -75.00000000000008527, 0.000000000000000000 ) ) ;
#1295 = VECTOR ( 'NONE', #505, 1000.000000000000000 ) ;
#1296 = ORIENTED_EDGE ( 'NONE', *, *, #6936, .T. ) ;
#1297 = DIRECTION ( 'NONE',  ( 0.000000000000000000, 0.000000000000000000, -1.000000000000000000 ) ) ;
#1298 = VERTEX_POINT ( 'NONE', #10465 ) ;
#1299 = EDGE_CURVE ( 'NONE', #13972, #8006, #4015, .T. ) ;
#1301 = DIRECTION ( 'NONE',  ( 1.000000000000000000, 0.000000000000000000, 0.000000000000000000 ) ) ;
#1300 = CIRCLE ( 'NONE', #6183, 5.000000000000004441 ) ;
#1302 = AXIS2_PLACEMENT_3D ( 'NONE', #4049, #7521, #1864 ) ;
#1303 = CARTESIAN_POINT ( 'NONE',  ( -0.2277608394786177770, 0.000000000000000000, 0.000000000000000000 ) ) ;
#1304 = CARTESIAN_POINT ( 'NONE',  ( 2.500000000000000000, -1.178949249685213863, 2.042000000000002924 ) ) ;
#1305 = CONICAL_SURFACE ( 'NONE', #9430, 0.8509999999999999787, 0.06981317007976602096 ) ;
#1306 = CARTESIAN_POINT ( 'NONE',  ( -30.00000000000002842, -25.00000000000000000, 250.0000000000000000 ) ) ;
#1307 = B_SPLINE_CURVE_WITH_KNOTS ( 'NONE', 3,
 ( #13617, #6813, #253, #11110, #11316 ),
 .UNSPECIFIED., .F., .F.,
 ( 4, 1, 4 ),
 ( 0.000000000000000000, 0.002309401076758505356, 0.004618802153517010713 ),
 .UNSPECIFIED. ) ;
#1308 = CARTESIAN_POINT ( 'NONE',  ( 303.3333333333333144, -15.00000000000000000, 225.1500000000000625 ) ) ;
#1309 = APPLICATION_PROTOCOL_DEFINITION ( 'draft international standard', 'automotive_design', 1998, #12033 ) ;
#1310 = CARTESIAN_POINT ( 'NONE',  ( -20.63749999999999574, 0.000000000000000000, -12.44999999999999929 ) ) ;
#1311 = AXIS2_PLACEMENT_3D ( 'NONE', #10625, #8428, #6047 ) ;
#1312 = VERTEX_POINT ( 'NONE', #2925 ) ;
#1313 = ORIENTED_EDGE ( 'NONE', *, *, #13261, .T. ) ;
#1314=STYLED_ITEM('',(#14410),#8329);
#1315 = ORIENTED_EDGE ( 'NONE', *, *, #12071, .F. ) ;
#1317 = DIRECTION ( 'NONE',  ( -0.000000000000000000, -0.000000000000000000, -1.000000000000000000 ) ) ;
#1316 = PRESENTATION_LAYER_ASSIGNMENT (  '', '', ( #10851 ) ) ;
#1318 = AXIS2_PLACEMENT_3D ( 'NONE', #6760, #2269, #6696 ) ;
#1319 = ORIENTED_EDGE ( 'NONE', *, *, #9416, .T. ) ;
#1320 = LINE ( 'NONE', #11483, #13363 ) ;
#1321 = EDGE_CURVE ( 'NONE', #13567, #5456, #13939, .T. ) ;
#1322 = FACE_OUTER_BOUND ( 'NONE', #10618, .T. ) ;
#1323 = EDGE_CURVE ( 'NONE', #3167, #3720, #9507, .T. ) ;
#1324 = FACE_OUTER_BOUND ( 'NONE', #13084, .T. ) ;
#1325 = CIRCLE ( 'NONE', #11073, 2.649999999999985700 ) ;
#1326 = VECTOR ( 'NONE', #5102, 1000.000000000000000 ) ;
#1327 = CARTESIAN_POINT ( 'NONE',  ( -1.799999999999996048, 1.224646799147353059E-15, 9.999999999999998224 ) ) ;
#1328 = DIRECTION ( 'NONE',  ( 1.000000000000000000, 0.000000000000000000, 0.000000000000000000 ) ) ;
#1329 = CARTESIAN_POINT ( 'NONE',  ( 1.800000000000001155, 0.000000000000000000, -13.29999999999999893 ) ) ;
#1330 = CARTESIAN_POINT ( 'NONE',  ( 1.999999999999994893, 0.000000000000000000, 0.000000000000000000 ) ) ;
#1331 = EDGE_CURVE ( 'NONE', #11674, #5306, #12710, .T. ) ;
#1332 = VERTEX_POINT ( 'NONE', #4961 ) ;
#1333 = DIRECTION ( 'NONE',  ( 0.000000000000000000, 1.000000000000000000, 0.000000000000000000 ) ) ;
#1334 = ADVANCED_FACE ( 'NONE', ( #13791, #8424 ), #3863, .F. ) ;
#1335 = CARTESIAN_POINT ( 'NONE',  ( -2.171643655288372443, 3.365003104552320767, 2.541098841762897165E-18 ) ) ;
#1336 = VECTOR ( 'NONE', #10698, 1000.000000000000000 ) ;
#1337 = DIRECTION ( 'NONE',  ( 1.007709689656716815E-16, 1.000000000000000000, 3.606821995490527259E-15 ) ) ;
#1338 = VERTEX_POINT ( 'NONE', #3943 ) ;
#1339 = DIRECTION ( 'NONE',  ( -1.000000000000000000, -0.000000000000000000, -0.000000000000000000 ) ) ;
#1340 = FACE_OUTER_BOUND ( 'NONE', #8047, .T. ) ;
#1341 = DIRECTION ( 'NONE',  ( 0.000000000000000000, 0.000000000000000000, -1.000000000000000000 ) ) ;
#1342 = EDGE_CURVE ( 'NONE', #568, #2622, #13004, .T. ) ;
#1343 = EDGE_CURVE ( 'NONE', #6665, #8094, #10619, .T. ) ;
#1344 = EDGE_LOOP ( 'NONE', ( #12384, #12486, #11903, #8733 ) ) ;
#1345 = CIRCLE ( 'NONE', #11564, 0.5155456020628804703 ) ;
#1346 = CARTESIAN_POINT ( 'NONE',  ( 386.6666666666666288, -20.00000000000000000, 222.5000000000000853 ) ) ;
#1347 = PRODUCT ( 'aligner', 'aligner', '', ( #6175 ) ) ;
#1348 = EDGE_LOOP ( 'NONE', ( #3565, #1722 ) ) ;
#1349 = CARTESIAN_POINT ( 'NONE',  ( 203.5000000000000000, -85.00000000000007105, 180.0000000000000000 ) ) ;
#1350 = EDGE_CURVE ( 'NONE', #5388, #6497, #3002, .T. ) ;
#1351 = ORIENTED_EDGE ( 'NONE', *, *, #11461, .T. ) ;
#1352 = ORIENTED_EDGE ( 'NONE', *, *, #13379, .F. ) ;
#1353 = CARTESIAN_POINT ( 'NONE',  ( -314.9999999999999432, -105.0000000000000995, 40.00000000000000000 ) ) ;
#1354 = DIRECTION ( 'NONE',  ( -0.000000000000000000, -0.000000000000000000, -1.000000000000000000 ) ) ;
#1355 = APPLICATION_CONTEXT ( 'automotive_design' ) ;
#1356 = FACE_OUTER_BOUND ( 'NONE', #5395, .T. ) ;
#1357 = VECTOR ( 'NONE', #4551, 1000.000000000000114 ) ;
#1358 = DIRECTION ( 'NONE',  ( -1.000000000000000000, -0.000000000000000000, -0.000000000000000000 ) ) ;
#1359 = LINE ( 'NONE', #2456, #10238 ) ;
#1360 = CYLINDRICAL_SURFACE ( 'NONE', #13582, 2.500000000000002220 ) ;
#1361 = CARTESIAN_POINT ( 'NONE',  ( 4.198928548860774157, -0.8158838809860124996, -3.526471437616918170 ) ) ;
#1362 = ORIENTED_EDGE ( 'NONE', *, *, #7124, .T. ) ;
#1363 = ORIENTED_EDGE ( 'NONE', *, *, #4120, .F. ) ;
#1364 = CYLINDRICAL_SURFACE ( 'NONE', #3147, 2.649999999999985700 ) ;
#1365 = VERTEX_POINT ( 'NONE', #8283 ) ;
#1366 = CARTESIAN_POINT ( 'NONE',  ( 434.9999999999999432, 8.660254037844390851, 199.9990000000000236 ) ) ;
#1367 = CIRCLE ( 'NONE', #11787, 2.700000000000000622 ) ;
#1368 = CIRCLE ( 'NONE', #12741, 2.649999999999985700 ) ;
#1369 = ORIENTED_EDGE ( 'NONE', *, *, #12633, .F. ) ;
#1370 = FACE_OUTER_BOUND ( 'NONE', #7900, .T. ) ;
#1371 = ORIENTED_EDGE ( 'NONE', *, *, #13161, .F. ) ;
#1372 = CIRCLE ( 'NONE', #11351, 2.649999999999985700 ) ;
#1373 = DIRECTION ( 'NONE',  ( -0.000000000000000000, -0.000000000000000000, 1.000000000000000000 ) ) ;
#1374 = CARTESIAN_POINT ( 'NONE',  ( 299.9999999999999432, -95.00000000000008527, 186.2999999999999829 ) ) ;
#1375 = ORIENTED_EDGE ( 'NONE', *, *, #13935, .T. ) ;
#1376 = FILL_AREA_STYLE_COLOUR ( '', #2490 ) ;
#1377 = EDGE_CURVE ( 'NONE', #5028, #10577, #8861, .T. ) ;
#1378 = CARTESIAN_POINT ( 'NONE',  ( 5.200000000000002842, 0.000000000000000000, 2.500000000000000888 ) ) ;
#1379 =( NAMED_UNIT ( * ) PLANE_ANGLE_UNIT ( ) SI_UNIT ( $, .RADIAN. ) );
#1380 = CARTESIAN_POINT ( 'NONE',  ( 238.9999999999999432, -85.00000000000007105, 190.0000000000000000 ) ) ;
#1381 = VERTEX_POINT ( 'NONE', #6113 ) ;
#1382 = VERTEX_POINT ( 'NONE', #5186 ) ;
#1383 = EDGE_LOOP ( 'NONE', ( #345, #4105, #13861, #8280 ) ) ;
#1384 = CONICAL_SURFACE ( 'NONE', #6268, 2.055000000000000160, 0.7853981633974639331 ) ;
#1385 = DIRECTION ( 'NONE',  ( -0.000000000000000000, -0.000000000000000000, 1.000000000000000000 ) ) ;
#1386 = B_SPLINE_CURVE_WITH_KNOTS ( 'NONE', 3,
 ( #10306, #4807, #14074, #12843 ),
 .UNSPECIFIED., .F., .F.,
 ( 4, 4 ),
 ( 0.000000000000000000, 0.002452478801916361129 ),
 .UNSPECIFIED. ) ;
#1387 = VERTEX_POINT ( 'NONE', #9600 ) ;
#1388 = CARTESIAN_POINT ( 'NONE',  ( 2.000000000000001776, 0.000000000000000000, 0.000000000000000000 ) ) ;
#1389 = ORIENTED_EDGE ( 'NONE', *, *, #13899, .T. ) ;
#1390 = DIRECTION ( 'NONE',  ( 1.000000000000000000, 0.000000000000000000, 0.000000000000000000 ) ) ;
#1391 = EDGE_CURVE ( 'NONE', #13737, #2488, #10419, .T. ) ;
#1392 = LINE ( 'NONE', #3871, #9220 ) ;
#1393 = VECTOR ( 'NONE', #7157, 1000.000000000000000 ) ;
#1394 = CARTESIAN_POINT ( 'NONE',  ( 132.3499999999999659, -56.99999999999997158, 10.00000000000000000 ) ) ;
#1395 = MECHANICAL_DESIGN_GEOMETRIC_PRESENTATION_REPRESENTATION (  '', ( #10207 ), #1885 ) ;
#1396 = FILL_AREA_STYLE_COLOUR ( '', #8829 ) ;
#1397 = FACE_OUTER_BOUND ( 'NONE', #9178, .T. ) ;
#1398 = CARTESIAN_POINT ( 'NONE',  ( 0.000000000000000000, -1.178949249685218303, -2.041999999999998039 ) ) ;
#1399 = EDGE_CURVE ( 'NONE', #11692, #1387, #14170, .T. ) ;
#1400 = VERTEX_POINT ( 'NONE', #13069 ) ;
#1401 = ADVANCED_FACE ( 'NONE', ( #6687, #8934 ), #11047, .T. ) ;
#1402 = AXIS2_PLACEMENT_3D ( 'NONE', #12026, #2967, #14188 ) ;
#1403 = AXIS2_PLACEMENT_3D ( 'NONE', #4738, #1592, #4667 ) ;
#1404 = DIRECTION ( 'NONE',  ( -1.000000000000000000, 0.000000000000000000, 0.000000000000000000 ) ) ;
#1405 = DIRECTION ( 'NONE',  ( -1.000000000000000000, -0.000000000000000000, -0.000000000000000000 ) ) ;
#1406 = CARTESIAN_POINT ( 'NONE',  ( -294.9999999999999432, -75.00000000000008527, 39.99999999999997868 ) ) ;
#1407 = EDGE_LOOP ( 'NONE', ( #8578, #7757, #9815, #9066 ) ) ;
#1408 = AXIS2_PLACEMENT_3D ( 'NONE', #6574, #5477, #9911 ) ;
#1409 = DIRECTION ( 'NONE',  ( 0.000000000000000000, 0.000000000000000000, -1.000000000000000000 ) ) ;
#1410 =( GEOMETRIC_REPRESENTATION_CONTEXT ( 3 ) GLOBAL_UNCERTAINTY_ASSIGNED_CONTEXT ( ( #13197 ) ) GLOBAL_UNIT_ASSIGNED_CONTEXT ( ( #9062, #3423, #3835 ) ) REPRESENTATION_CONTEXT ( 'NONE', 'WORKASPACE' ) );
#1411 = DIRECTION ( 'NONE',  ( -1.000000000000000000, 0.000000000000000000, 0.000000000000000000 ) ) ;
#1412 = DIRECTION ( 'NONE',  ( 6.123233995736766036E-17, -1.000000000000000000, 0.000000000000000000 ) ) ;
#1413 = EDGE_CURVE ( 'NONE', #13509, #4208, #3762, .T. ) ;
#1414 = DIRECTION ( 'NONE',  ( -0.000000000000000000, -0.000000000000000000, -1.000000000000000000 ) ) ;
#1415 = EDGE_CURVE ( 'NONE', #6044, #3377, #11120, .T. ) ;
#1416 = VERTEX_POINT ( 'NONE', #3365 ) ;
#1417 = FACE_OUTER_BOUND ( 'NONE', #5088, .T. ) ;
#1418 = AXIS2_PLACEMENT_3D ( 'NONE', #10970, #3355, #2105 ) ;
#1419 = ORIENTED_EDGE ( 'NONE', *, *, #9116, .T. ) ;
#1420 = DIRECTION ( 'NONE',  ( -0.000000000000000000, 0.000000000000000000, 1.000000000000000000 ) ) ;
#1421 = AXIS2_PLACEMENT_3D ( 'NONE', #11093, #8974, #13750 ) ;
#1422 = EDGE_LOOP ( 'NONE', ( #10256, #6078 ) ) ;
#1423 = EDGE_LOOP ( 'NONE', ( #8180, #5861, #11249, #6169 ) ) ;
#1424 = CONICAL_SURFACE ( 'NONE', #9083, 2.500000000000002220, 1.029744260000002631 ) ;
#1425 = ADVANCED_BREP_SHAPE_REPRESENTATION ( '', ( #3853, #14039 ), #731 ) ;
#1426 = CARTESIAN_POINT ( 'NONE',  ( 434.9999999999999432, -8.660254037844389075, 199.9990000000000236 ) ) ;
#1427 = EDGE_CURVE ( 'NONE', #12703, #13122, #7623, .T. ) ;
#1428 = EDGE_CURVE ( 'NONE', #11776, #12690, #14223, .T. ) ;
#1429 = CARTESIAN_POINT ( 'NONE',  ( -0.1756481739660520902, 4.720212674038980261, -3.469390959564065291 ) ) ;
#1430 = DIRECTION ( 'NONE',  ( 0.8949343913984143528, -1.557891129246500526E-15, 0.4461977533474922875 ) ) ;
#1431 = EDGE_CURVE ( 'NONE', #1100, #50, #10979, .T. ) ;
#1432 = DIRECTION ( 'NONE',  ( 0.000000000000000000, 1.000000000000000000, 1.086455722314322026E-16 ) ) ;
#1433 = DIRECTION ( 'NONE',  ( 1.000000000000000000, 0.000000000000000000, 0.000000000000000000 ) ) ;
#1434 = FACE_OUTER_BOUND ( 'NONE', #10121, .T. ) ;
#1435 = CIRCLE ( 'NONE', #4922, 10.00000000000000000 ) ;
#1436 = CARTESIAN_POINT ( 'NONE',  ( 137.6499999999999488, -36.99999999999997868, 10.00000000000000178 ) ) ;
#1437 = CONTEXT_DEPENDENT_SHAPE_REPRESENTATION ( #3540, #774 ) ;
#1438 = PRODUCT_DEFINITION_FORMATION_WITH_SPECIFIED_SOURCE ( 'ANY', '', #7946, .NOT_KNOWN. ) ;
#1439 = ORIENTED_EDGE ( 'NONE', *, *, #11588, .F. ) ;
#1440 = VECTOR ( 'NONE', #9291, 1000.000000000000114 ) ;
#1441 = ORIENTED_EDGE ( 'NONE', *, *, #12534, .T. ) ;
#1442 = CARTESIAN_POINT ( 'NONE',  ( 470.0000000000000000, -25.00000000000000000, 250.0000000000000000 ) ) ;
#1443 = EDGE_LOOP ( 'NONE', ( #5714, #13976, #8402, #3936 ) ) ;
#1444 = CARTESIAN_POINT ( 'NONE',  ( 4.999999999999999112, 8.660254037844390851, 210.0000000000000000 ) ) ;
#1445 = VECTOR ( 'NONE', #3310, 1000.000000000000000 ) ;
#1446 = ORIENTED_EDGE ( 'NONE', *, *, #2292, .T. ) ;
#1447 = DIRECTION ( 'NONE',  ( -1.000000000000000000, 0.000000000000000000, 0.000000000000000000 ) ) ;
#1448 = VERTEX_POINT ( 'NONE', #12062 ) ;
#1449 = CYLINDRICAL_SURFACE ( 'NONE', #13340, 2.649999999999985700 ) ;
#1450 = DIRECTION ( 'NONE',  ( 0.000000000000000000, 0.000000000000000000, 1.000000000000000000 ) ) ;
#1451 = DIRECTION ( 'NONE',  ( 0.000000000000000000, 0.000000000000000000, -1.000000000000000000 ) ) ;
#1452 = VERTEX_POINT ( 'NONE', #861 ) ;
#1453 = DIRECTION ( 'NONE',  ( 1.000000000000000000, 0.000000000000000000, 0.000000000000000000 ) ) ;
#1454 = DIRECTION ( 'NONE',  ( 0.000000000000000000, 0.000000000000000000, 1.000000000000000000 ) ) ;
#1455 = SURFACE_STYLE_FILL_AREA ( #7183 ) ;
#1456 = FACE_BOUND ( 'NONE', #10648, .T. ) ;
#1457 = ORIENTED_EDGE ( 'NONE', *, *, #13975, .T. ) ;
#1458 = ORIENTED_EDGE ( 'NONE', *, *, #9714, .T. ) ;
#1459 = ORIENTED_EDGE ( 'NONE', *, *, #6313, .T. ) ;
#1460 = ADVANCED_FACE ( 'NONE', ( #5530 ), #8865, .F. ) ;
#1461 = LINE ( 'NONE', #5971, #12295 ) ;
#1462 = EDGE_LOOP ( 'NONE', ( #7055, #3073, #3390, #9366, #2015, #2649 ) ) ;
#1463 = ORIENTED_EDGE ( 'NONE', *, *, #4765, .F. ) ;
#1464 = FACE_OUTER_BOUND ( 'NONE', #495, .T. ) ;
#1465 = CARTESIAN_POINT ( 'NONE',  ( 0.000000000000000000, 0.000000000000000000, 190.0000000000000000 ) ) ;
#1466 = DIRECTION ( 'NONE',  ( -0.000000000000000000, -0.000000000000000000, 1.000000000000000000 ) ) ;
#1467 = DIRECTION ( 'NONE',  ( 0.000000000000000000, 0.000000000000000000, -1.000000000000000000 ) ) ;
#1468 = CARTESIAN_POINT ( 'NONE',  ( 1.800000000000001155, 1.628780242865979758E-15, 13.29999999999999893 ) ) ;
#1469 = CARTESIAN_POINT ( 'NONE',  ( 1.567478505476134606E-15, 4.618802153517012066, -5.000000000000000000 ) ) ;
#1470 = PRODUCT_DEFINITION_SHAPE ( 'NONE', 'NONE',  #14315 ) ;
#1471 = PLANE ( 'NONE',  #12390 ) ;
#1472 = ORIENTED_EDGE ( 'NONE', *, *, #302, .F. ) ;
#1473 = CARTESIAN_POINT ( 'NONE',  ( 53.33333333333330017, -20.00000000000000000, -225.1500000000000625 ) ) ;
#1474 = CARTESIAN_POINT ( 'NONE',  ( 3.900000000000000799, 0.000000000000000000, 0.000000000000000000 ) ) ;
#1475 = CIRCLE ( 'NONE', #5894, 2.500000000000002220 ) ;
#1476 = CARTESIAN_POINT ( 'NONE',  ( 181.0000000000000000, 8.660254037844390851, 200.0000000000000000 ) ) ;
#1477 = ORIENTED_EDGE ( 'NONE', *, *, #2537, .T. ) ;
#1478 = ADVANCED_FACE ( 'NONE', ( #2117 ), #2261, .F. ) ;
#1479 = LINE ( 'NONE', #10272, #3517 ) ;
#1480 = EDGE_CURVE ( 'NONE', #11371, #2677, #11299, .T. ) ;
#1481 = DIRECTION ( 'NONE',  ( 0.000000000000000000, 0.000000000000000000, 1.000000000000000000 ) ) ;
#1482 = DIRECTION ( 'NONE',  ( 1.000000000000000000, 0.000000000000000000, 0.000000000000000000 ) ) ;
#1483 = DIRECTION ( 'NONE',  ( 1.000000000000000000, 0.000000000000000000, 0.000000000000000000 ) ) ;
#1484 = EDGE_LOOP ( 'NONE', ( #13326, #12481 ) ) ;
#1485 = FACE_OUTER_BOUND ( 'NONE', #5885, .T. ) ;
#1486 = CARTESIAN_POINT ( 'NONE',  ( 219.9999999999999147, -85.00000000000009948, -17.55500000000000327 ) ) ;
#1487 = EDGE_LOOP ( 'NONE', ( #13050, #13231, #569, #1131 ) ) ;
#1489 = EDGE_CURVE ( 'NONE', #11495, #5325, #5454, .T. ) ;
#1488 = CARTESIAN_POINT ( 'NONE',  ( 140.0000000000000000, -95.00000000000008527, -190.0000000000000000 ) ) ;
#1490 = PRODUCT_RELATED_PRODUCT_CATEGORY ( 'part', '', ( #173 ) ) ;
#1491 = CARTESIAN_POINT ( 'NONE',  ( -0.5449313310646672903, -4.304185902836978883, -3.316620875263469159 ) ) ;
#1492 = CYLINDRICAL_SURFACE ( 'NONE', #2708, 4.250000000000000000 ) ;
#1493 = LINE ( 'NONE', #2671, #6042 ) ;
#1494 = CARTESIAN_POINT ( 'NONE',  ( -2.059999999999998721, 2.522772406243545965E-16, -0.3080913168122742518 ) ) ;
#1495 = FACE_OUTER_BOUND ( 'NONE', #8735, .T. ) ;
#1496 = ADVANCED_FACE ( 'NONE', ( #10029 ), #9955, .F. ) ;
#1497 = CARTESIAN_POINT ( 'NONE',  ( 2.500000000000000000, 2.357898499370433054, -1.951563910473907981E-15 ) ) ;
#1498 = ITEM_DEFINED_TRANSFORMATION ( 'NONE', 'NONE', #12563,  #14039 ) ;
#1499 = ORIENTED_EDGE ( 'NONE', *, *, #14078, .F. ) ;
#1500 = ORIENTED_EDGE ( 'NONE', *, *, #7562, .F. ) ;
#1501 = EDGE_CURVE ( 'NONE', #7291, #7986, #5623, .T. ) ;
#1502 = ADVANCED_FACE ( 'NONE', ( #3222 ), #1424, .F. ) ;
#1503 = CARTESIAN_POINT ( 'NONE',  ( 93.00000000000000000, 8.660254037844390851, 200.0000000000000000 ) ) ;
#1504 = AXIS2_PLACEMENT_3D ( 'NONE', #9296, #13632, #11540 ) ;
#1505 = EDGE_LOOP ( 'NONE', ( #3985, #10939 ) ) ;
#1506 = AXIS2_PLACEMENT_3D ( 'NONE', #11230, #240, #8839 ) ;
#1507 = CARTESIAN_POINT ( 'NONE',  ( 3.700000000000000178, 0.000000000000000000, 0.000000000000000000 ) ) ;
#1508 = ORIENTED_EDGE ( 'NONE', *, *, #7566, .T. ) ;
#1509 = DIRECTION ( 'NONE',  ( 0.000000000000000000, 0.000000000000000000, -1.000000000000000000 ) ) ;
#1510 = ORIENTED_EDGE ( 'NONE', *, *, #1288, .F. ) ;
#1512 = EDGE_CURVE ( 'NONE', #4493, #865, #13215, .T. ) ;
#1511 = DIRECTION ( 'NONE',  ( 1.000000000000000000, 0.000000000000000000, 0.000000000000000000 ) ) ;
#1513 = DIRECTION ( 'NONE',  ( -1.000000000000000000, 0.000000000000000000, 0.000000000000000000 ) ) ;
#1514 = VERTEX_POINT ( 'NONE', #3077 ) ;
#1515 = CARTESIAN_POINT ( 'NONE',  ( 2.740000000000000213, -0.9838866223905676778, 0.5149999999999995692 ) ) ;
#1516 = CARTESIAN_POINT ( 'NONE',  ( -1.149515148933662080E-15, -4.736529461166056443, -3.681130640444383317 ) ) ;
#1517 = AXIS2_PLACEMENT_3D ( 'NONE', #11311, #5715, #11102 ) ;
#1518 =( NAMED_UNIT ( * ) SI_UNIT ( $, .STERADIAN. ) SOLID_ANGLE_UNIT ( ) );
#1519 = DIRECTION ( 'NONE',  ( 0.000000000000000000, 0.000000000000000000, -1.000000000000000000 ) ) ;
#1520 = APPLICATION_PROTOCOL_DEFINITION ( 'draft international standard', 'automotive_design', 1998, #8311 ) ;
#1521 = VECTOR ( 'NONE', #4856, 1000.000000000000000 ) ;
#1522 = DIRECTION ( 'NONE',  ( -1.000000000000000000, 0.000000000000000000, 0.000000000000000000 ) ) ;
#1523 = ORIENTED_EDGE ( 'NONE', *, *, #8262, .F. ) ;
#1524 = EDGE_CURVE ( 'NONE', #6598, #3716, #12128, .T. ) ;
#1525 = EDGE_LOOP ( 'NONE', ( #12096, #1587 ) ) ;
#1526 = ORIENTED_EDGE ( 'NONE', *, *, #263, .T. ) ;
#1527 = EDGE_CURVE ( 'NONE', #2397, #11346, #11181, .T. ) ;
#1528 = DIRECTION ( 'NONE',  ( 0.000000000000000000, 0.000000000000000000, -1.000000000000000000 ) ) ;
#1529 = AXIS2_PLACEMENT_3D ( 'NONE', #2301, #4549, #6656 ) ;
#1530 = AXIS2_PLACEMENT_3D ( 'NONE', #9386, #12937, #7060 ) ;
#1531 = EDGE_LOOP ( 'NONE', ( #3203, #13066, #4904 ) ) ;
#1532 = DIRECTION ( 'NONE',  ( -0.000000000000000000, -0.000000000000000000, -1.000000000000000000 ) ) ;
#1533 = ORIENTED_EDGE ( 'NONE', *, *, #302, .T. ) ;
#1534 = CARTESIAN_POINT ( 'NONE',  ( -5.000000000000000888, 8.660254037844390851, 205.0000000000000284 ) ) ;
#1535 = ADVANCED_FACE ( 'NONE', ( #6964 ), #10723, .T. ) ;
#1536 = VECTOR ( 'NONE', #3721, 1000.000000000000000 ) ;
#1537 = CARTESIAN_POINT ( 'NONE',  ( 0.000000000000000000, 0.000000000000000000, -186.0000000000000000 ) ) ;
#1538 = VECTOR ( 'NONE', #2570, 1000.000000000000000 ) ;
#1539 = DIRECTION ( 'NONE',  ( 0.000000000000000000, 1.000000000000000000, 0.000000000000000000 ) ) ;
#1540 = AXIS2_PLACEMENT_3D ( 'NONE', #8940, #1163, #13353 ) ;
#1541 = DIRECTION ( 'NONE',  ( 0.000000000000000000, 0.000000000000000000, 1.000000000000000000 ) ) ;
#1542 = CARTESIAN_POINT ( 'NONE',  ( 134.9999999999999432, -36.99999999999997868, 10.00000000000000000 ) ) ;
#1543 = VECTOR ( 'NONE', #13285, 1000.000000000000000 ) ;
#1544 = ORIENTED_EDGE ( 'NONE', *, *, #720, .F. ) ;
#1545 = AXIS2_PLACEMENT_3D ( 'NONE', #4006, #10533, #9520 ) ;
#1546 = CARTESIAN_POINT ( 'NONE',  ( 21.00000000000000355, 0.000000000000000000, 0.000000000000000000 ) ) ;
#1547 = DIRECTION ( 'NONE',  ( 0.000000000000000000, 0.000000000000000000, 1.000000000000000000 ) ) ;
#1548 = CONICAL_SURFACE ( 'NONE', #12457, 2.055000000000000160, 0.7853981633974633780 ) ;
#1549 = DIRECTION ( 'NONE',  ( 1.000000000000000000, 0.000000000000000000, 0.000000000000000000 ) ) ;
#1550 = ORIENTED_EDGE ( 'NONE', *, *, #2851, .F. ) ;
#1551 = CIRCLE ( 'NONE', #6442, 2.649999999999985700 ) ;
#1552 = FACE_OUTER_BOUND ( 'NONE', #13347, .T. ) ;
#1553 = EDGE_CURVE ( 'NONE', #8456, #8038, #4796, .T. ) ;
#1554 = DIRECTION ( 'NONE',  ( 1.000000000000000000, 0.000000000000000000, 0.000000000000000000 ) ) ;
#1555 = DIRECTION ( 'NONE',  ( 0.000000000000000000, 0.000000000000000000, 1.000000000000000000 ) ) ;
#1556 = DIRECTION ( 'NONE',  ( 1.000000000000000000, 0.000000000000000000, -0.000000000000000000 ) ) ;
#1557 = AXIS2_PLACEMENT_3D ( 'NONE', #464, #13905, #5078 ) ;
#1558 = VERTEX_POINT ( 'NONE', #119 ) ;
#1559 = AXIS2_PLACEMENT_3D ( 'NONE', #9022, #11654, #13798 ) ;
#1560 = CARTESIAN_POINT ( 'NONE',  ( -1.144235203016679359, -3.958177651039096911, -0.09382832055446428676 ) ) ;
#1561 = DIRECTION ( 'NONE',  ( 1.000000000000000000, 0.000000000000000000, 0.000000000000000000 ) ) ;
#1562 = ORIENTED_EDGE ( 'NONE', *, *, #10674, .F. ) ;
#1563 = FACE_BOUND ( 'NONE', #12336, .T. ) ;
#1564 = CARTESIAN_POINT ( 'NONE',  ( -1.287237434361707233, -3.875615274277397937, -3.430618716626816500 ) ) ;
#1565 =( REPRESENTATION_RELATIONSHIP ('NONE','NONE', #11251, #10314 ) REPRESENTATION_RELATIONSHIP_WITH_TRANSFORMATION ( #169 )SHAPE_REPRESENTATION_RELATIONSHIP( ) );
#1566 = CARTESIAN_POINT ( 'NONE',  ( -5.560781378645575757, 6.809993116116508640E-16, -4.000000000000000000 ) ) ;
#1567 = DIRECTION ( 'NONE',  ( 1.000000000000000000, 0.000000000000000000, 0.000000000000000000 ) ) ;
#1568 = LINE ( 'NONE', #1643, #3080 ) ;
#1569 = CARTESIAN_POINT ( 'NONE',  ( -140.0000000000000000, -75.00000000000008527, 30.00000000000000000 ) ) ;
#1570 = DIRECTION ( 'NONE',  ( 0.000000000000000000, 0.000000000000000000, -1.000000000000000000 ) ) ;
#1571 = ITEM_DEFINED_TRANSFORMATION ( 'NONE', 'NONE', #25,  #14039 ) ;
#1572 = ORIENTED_EDGE ( 'NONE', *, *, #3032, .F. ) ;
#1573 = EDGE_LOOP ( 'NONE', ( #1925, #12567, #6022, #193 ) ) ;
#1574 = EDGE_CURVE ( 'NONE', #3366, #4058, #6753, .T. ) ;
#1575 = LINE ( 'NONE', #2902, #5911 ) ;
#1576 = EDGE_CURVE ( 'NONE', #8786, #486, #1227, .T. ) ;
#1577 = ORIENTED_EDGE ( 'NONE', *, *, #11810, .T. ) ;
#1578 = DIRECTION ( 'NONE',  ( 0.000000000000000000, 0.000000000000000000, 1.000000000000000000 ) ) ;
#1579 = CARTESIAN_POINT ( 'NONE',  ( 470.0000000000000000, 15.00000000000000000, 205.0000000000000284 ) ) ;
#1580 = ORIENTED_EDGE ( 'NONE', *, *, #6064, .T. ) ;
#1581 = DIRECTION ( 'NONE',  ( -0.000000000000000000, 1.000000000000000000, -0.000000000000000000 ) ) ;
#1582 = ORIENTED_EDGE ( 'NONE', *, *, #8645, .T. ) ;
#1583 = AXIS2_PLACEMENT_3D ( 'NONE', #902, #8465, #6297 ) ;
#1584 = FACE_OUTER_BOUND ( 'NONE', #8667, .T. ) ;
#1585 = PRODUCT_DEFINITION_SHAPE ( 'NONE', 'NONE',  #14333 ) ;
#1586 = DIRECTION ( 'NONE',  ( 1.000000000000000000, 0.000000000000000000, 0.000000000000000000 ) ) ;
#1587 = ORIENTED_EDGE ( 'NONE', *, *, #6484, .T. ) ;
#1588 = UNCERTAINTY_MEASURE_WITH_UNIT (LENGTH_MEASURE( 1.000000000000000082E-05 ), #2896, 'distance_accuracy_value', 'NONE');
#1589 =( LENGTH_UNIT ( ) NAMED_UNIT ( * ) SI_UNIT ( .MILLI., .METRE. ) );
#1590 = CARTESIAN_POINT ( 'NONE',  ( 259.0000000000000000, -8.660254037844389075, 200.0000000000000000 ) ) ;
#1591 =( NAMED_UNIT ( * ) SI_UNIT ( $, .STERADIAN. ) SOLID_ANGLE_UNIT ( ) );
#1592 = DIRECTION ( 'NONE',  ( 0.000000000000000000, -1.000000000000000000, 0.000000000000000000 ) ) ;
#1593 = SHAPE_DEFINITION_REPRESENTATION ( #4610, #5332 ) ;
#1594 = CARTESIAN_POINT ( 'NONE',  ( 206.1500000000000057, -85.00000000000007105, 55.00000000000001421 ) ) ;
#1595 = ORIENTED_EDGE ( 'NONE', *, *, #3891, .F. ) ;
#1596 = AXIS2_PLACEMENT_3D ( 'NONE', #12454, #5918, #11436 ) ;
#1597 = EDGE_CURVE ( 'NONE', #3594, #13983, #12100, .T. ) ;
#1598 = ORIENTED_EDGE ( 'NONE', *, *, #5147, .T. ) ;
#1599 = PRODUCT_DEFINITION ( 'UNKNOWN', '', #12106, #8270 ) ;
#1600 = VERTEX_POINT ( 'NONE', #7966 ) ;
#1601 = CARTESIAN_POINT ( 'NONE',  ( 3.680118525130245732, -2.494084732383344605, -0.3507732604232533524 ) ) ;
#1602 = EDGE_CURVE ( 'NONE', #1381, #10838, #1911, .T. ) ;
#1603 = EDGE_LOOP ( 'NONE', ( #9481, #9467, #7447, #1731 ) ) ;
#1604 = LINE ( 'NONE', #5975, #7116 ) ;
#1605 = ORIENTED_EDGE ( 'NONE', *, *, #12867, .T. ) ;
#1606 = LINE ( 'NONE', #4020, #8260 ) ;
#1607 = FILL_AREA_STYLE ('',( #7136 ) ) ;
#1608 = CARTESIAN_POINT ( 'NONE',  ( 0.000000000000000000, 0.000000000000000000, 250.0000000000000000 ) ) ;
#1609 = EDGE_CURVE ( 'NONE', #8612, #3475, #7899, .T. ) ;
#1610 = EDGE_CURVE ( 'NONE', #328, #11751, #2402, .T. ) ;
#1611 = FACE_OUTER_BOUND ( 'NONE', #2638, .T. ) ;
#1612 = AXIS2_PLACEMENT_3D ( 'NONE', #11512, #8386, #13754 ) ;
#1613 = EDGE_CURVE ( 'NONE', #13461, #8622, #8044, .T. ) ;
#1614 = EDGE_CURVE ( 'NONE', #12208, #6338, #5662, .T. ) ;
#1615 = AXIS2_PLACEMENT_3D ( 'NONE', #13114, #843, #12984 ) ;
#1616 = DIRECTION ( 'NONE',  ( 0.000000000000000000, 1.000000000000000000, 0.000000000000000000 ) ) ;
#1617 = CARTESIAN_POINT ( 'NONE',  ( 0.2500000000000002220, 0.000000000000000000, 0.000000000000000000 ) ) ;
#1618 = ORIENTED_EDGE ( 'NONE', *, *, #5421, .F. ) ;
#1619 = ORIENTED_EDGE ( 'NONE', *, *, #4025, .T. ) ;
#1620 = SURFACE_STYLE_FILL_AREA ( #2512 ) ;
#1621 = VECTOR ( 'NONE', #6943, 1000.000000000000000 ) ;
#1622 = DIRECTION ( 'NONE',  ( -0.000000000000000000, -0.000000000000000000, -1.000000000000000000 ) ) ;
#1623 = CYLINDRICAL_SURFACE ( 'NONE', #13952, 11.05000000000000071 ) ;
#1624 = CARTESIAN_POINT ( 'NONE',  ( 0.000000000000000000, 0.000000000000000000, -186.0000000000000000 ) ) ;
#1625 = VERTEX_POINT ( 'NONE', #6894 ) ;
#1626 = CARTESIAN_POINT ( 'NONE',  ( -302.4999999999999432, -75.00000000000008527, 329.9999999999999432 ) ) ;
#1627 = FACE_OUTER_BOUND ( 'NONE', #2552, .T. ) ;
#1628 = CARTESIAN_POINT ( 'NONE',  ( 264.0000000000000000, 0.000000000000000000, 188.0000000000000000 ) ) ;
#1629 = AXIS2_PLACEMENT_3D ( 'NONE', #8903, #3394, #3334 ) ;
#1630 = DIRECTION ( 'NONE',  ( -1.000000000000000000, 0.000000000000000000, -0.000000000000000000 ) ) ;
#1631 = CARTESIAN_POINT ( 'NONE',  ( -134.9999999999999716, 45.00000000000001421, 30.00000000000000000 ) ) ;
#1632 = APPLICATION_CONTEXT ( 'automotive_design' ) ;
#1633 = VECTOR ( 'NONE', #12005, 1000.000000000000000 ) ;
#1634 = EDGE_LOOP ( 'NONE', ( #5750, #1743, #13000, #57 ) ) ;
#1635 = CARTESIAN_POINT ( 'NONE',  ( -1.654252653721913102, -3.663718938583024443, -0.01223254789874440342 ) ) ;
#1636 = EDGE_CURVE ( 'NONE', #3478, #12287, #8116, .T. ) ;
#1637 = CARTESIAN_POINT ( 'NONE',  ( 222.0549999999999216, -85.00000000000009948, -18.00000000000000355 ) ) ;
#1638 = CIRCLE ( 'NONE', #1408, 2.649999999999985700 ) ;
#1639 = ORIENTED_EDGE ( 'NONE', *, *, #4832, .T. ) ;
#1640 = CARTESIAN_POINT ( 'NONE',  ( 2.500000000000000000, 0.000000000000000000, 0.000000000000000000 ) ) ;
#1641 =( GEOMETRIC_REPRESENTATION_CONTEXT ( 3 ) GLOBAL_UNCERTAINTY_ASSIGNED_CONTEXT ( ( #12772 ) ) GLOBAL_UNIT_ASSIGNED_CONTEXT ( ( #9225, #2846, #1518 ) ) REPRESENTATION_CONTEXT ( 'NONE', 'WORKASPACE' ) );
#1642 = FACE_OUTER_BOUND ( 'NONE', #13415, .T. ) ;
#1643 = CARTESIAN_POINT ( 'NONE',  ( 386.6666666666666288, -20.00000000000000000, -225.1500000000000625 ) ) ;
#1644 = PLANE ( 'NONE',  #356 ) ;
#1645 =( NAMED_UNIT ( * ) PLANE_ANGLE_UNIT ( ) SI_UNIT ( $, .RADIAN. ) );
#1646 = CARTESIAN_POINT ( 'NONE',  ( 0.1750025118121568690, 4.719839900820621104, -3.469254087858248070 ) ) ;
#1647 = ITEM_DEFINED_TRANSFORMATION ( 'NONE', 'NONE', #10946,  #14039 ) ;
#1648 = VECTOR ( 'NONE', #2392, 1000.000000000000000 ) ;
#1649 = CIRCLE ( 'NONE', #473, 5.000000000000004441 ) ;
#1650 = ORIENTED_EDGE ( 'NONE', *, *, #13490, .T. ) ;
#1651 = FACE_BOUND ( 'NONE', #10444, .T. ) ;
#1652 =( GEOMETRIC_REPRESENTATION_CONTEXT ( 3 ) GLOBAL_UNCERTAINTY_ASSIGNED_CONTEXT ( ( #11030 ) ) GLOBAL_UNIT_ASSIGNED_CONTEXT ( ( #8033, #5002, #8247 ) ) REPRESENTATION_CONTEXT ( 'NONE', 'WORKASPACE' ) );
#1653 = ORIENTED_EDGE ( 'NONE', *, *, #8448, .T. ) ;
#1654 = DIRECTION ( 'NONE',  ( 1.000000000000000000, 0.000000000000000000, 0.000000000000000000 ) ) ;
#1655 = CYLINDRICAL_SURFACE ( 'NONE', #5562, 5.000000000000004441 ) ;
#1656 = ORIENTED_EDGE ( 'NONE', *, *, #12195, .T. ) ;
#1657 = CARTESIAN_POINT ( 'NONE',  ( -4.198928548860774157, 0.8158838809860065044, -3.526471437616918170 ) ) ;
#1658 = ORIENTED_EDGE ( 'NONE', *, *, #3196, .F. ) ;
#1659 = CARTESIAN_POINT ( 'NONE',  ( 136.6666666666666288, -14.99999999999999822, 219.8500000000001080 ) ) ;
#1660 = FACE_OUTER_BOUND ( 'NONE', #13209, .T. ) ;
#1662 = VERTEX_POINT ( 'NONE', #325 ) ;
#1661 = VECTOR ( 'NONE', #6856, 1000.000000000000000 ) ;
#1663 = SURFACE_STYLE_FILL_AREA ( #7326 ) ;
#1664 = ADVANCED_FACE ( 'NONE', ( #5875 ), #13416, .F. ) ;
#1665 = CARTESIAN_POINT ( 'NONE',  ( 469.9999999999998863, -25.00000000000000000, 169.9999999999999716 ) ) ;
#1666 = AXIS2_PLACEMENT_3D ( 'NONE', #2592, #13525, #7013 ) ;
#1667 = MECHANICAL_DESIGN_GEOMETRIC_PRESENTATION_REPRESENTATION (  '', ( #8148 ), #9795 ) ;
#1668 = VECTOR ( 'NONE', #2684, 1000.000000000000000 ) ;
#1669 = SURFACE_SIDE_STYLE ('',( #1455 ) ) ;
#1670 = CONTEXT_DEPENDENT_SHAPE_REPRESENTATION ( #135, #2525 ) ;
#1671 = CARTESIAN_POINT ( 'NONE',  ( 4.000000000000000000, 2.309401076758497151, -5.000000000000000000 ) ) ;
#1672 = EDGE_LOOP ( 'NONE', ( #11529, #10002, #6110, #12494 ) ) ;
#1673 = EDGE_LOOP ( 'NONE', ( #9501, #13329, #5600, #2944 ) ) ;
#1674 = DIRECTION ( 'NONE',  ( 0.000000000000000000, 0.000000000000000000, 1.000000000000000000 ) ) ;
#1676 = CIRCLE ( 'NONE', #9804, 5.500000000000005329 ) ;
#1675 = CIRCLE ( 'NONE', #11651, 2.649999999999985700 ) ;
#1677 = VERTEX_POINT ( 'NONE', #10297 ) ;
#1678 = CARTESIAN_POINT ( 'NONE',  ( 206.0000000000000284, -85.00000000000007105, 180.0000000000000000 ) ) ;
#1679 = ADVANCED_FACE ( 'NONE', ( #2667 ), #2934, .T. ) ;
#1680 = ORIENTED_EDGE ( 'NONE', *, *, #11034, .F. ) ;
#1681 = DIRECTION ( 'NONE',  ( 0.000000000000000000, -1.224646799147353454E-16, 1.000000000000000000 ) ) ;
#1682 = VERTEX_POINT ( 'NONE', #1444 ) ;
#1683 = CARTESIAN_POINT ( 'NONE',  ( 0.000000000000000000, 0.000000000000000000, 0.000000000000000000 ) ) ;
#1684 = UNCERTAINTY_MEASURE_WITH_UNIT (LENGTH_MEASURE( 1.000000000000000082E-05 ), #1589, 'distance_accuracy_value', 'NONE');
#1685 = LINE ( 'NONE', #12503, #3446 ) ;
#1686 = PLANE ( 'NONE',  #10340 ) ;
#1687 = EDGE_CURVE ( 'NONE', #8236, #6756, #13958, .T. ) ;
#1688 = PRODUCT_RELATED_PRODUCT_CATEGORY ( 'part', '', ( #2407 ) ) ;
#1689 = DIRECTION ( 'NONE',  ( -1.000000000000000000, 0.000000000000000000, 0.000000000000000000 ) ) ;
#1690 = SURFACE_SIDE_STYLE ('',( #289 ) ) ;
#1691 = CARTESIAN_POINT ( 'NONE',  ( -294.9999999999999432, -75.00000000000008527, 354.1421356237308942 ) ) ;
#1692 = ORIENTED_EDGE ( 'NONE', *, *, #11438, .T. ) ;
#1693 = ORIENTED_EDGE ( 'NONE', *, *, #13590, .F. ) ;
#1694 = EDGE_CURVE ( 'NONE', #4527, #2366, #7834, .T. ) ;
#1695 = EDGE_CURVE ( 'NONE', #7212, #9436, #2619, .T. ) ;
#1696 = LINE ( 'NONE', #8592, #14186 ) ;
#1697 = EDGE_CURVE ( 'NONE', #2635, #10395, #4703, .T. ) ;
#1698 = ORIENTED_EDGE ( 'NONE', *, *, #11906, .T. ) ;
#1699 = CARTESIAN_POINT ( 'NONE',  ( 0.3226060873438244547, -2.189154565102686245, -0.5150000000000000133 ) ) ;
#1700 = DIRECTION ( 'NONE',  ( 0.000000000000000000, 0.4999999999999993339, -0.8660254037844390407 ) ) ;
#1701 = FACE_OUTER_BOUND ( 'NONE', #8205, .T. ) ;
#1702 = ORIENTED_EDGE ( 'NONE', *, *, #4765, .T. ) ;
#1703 = CARTESIAN_POINT ( 'NONE',  ( 219.9999999999999716, -85.00000000000007105, 170.0000000000000000 ) ) ;
#1704 = FACE_OUTER_BOUND ( 'NONE', #9597, .T. ) ;
#1705 = DIRECTION ( 'NONE',  ( 1.000000000000000000, 0.000000000000000000, 0.000000000000000000 ) ) ;
#1706 = DIRECTION ( 'NONE',  ( 1.000000000000000000, 0.000000000000000000, 0.000000000000000000 ) ) ;
#1707 = CARTESIAN_POINT ( 'NONE',  ( 219.9999999999999716, -20.00000000000000000, -219.8500000000001080 ) ) ;
#1708 = VERTEX_POINT ( 'NONE', #399 ) ;
#1709 = DIRECTION ( 'NONE',  ( -1.000000000000000000, 2.312964634635743450E-16, 0.000000000000000000 ) ) ;
#1710 = PRODUCT_DEFINITION_SHAPE ( 'NONE', 'NONE',  #14364 ) ;
#1711 = ADVANCED_FACE ( 'NONE', ( #9069 ), #13491, .F. ) ;
#1712 = DIRECTION ( 'NONE',  ( 0.000000000000000000, -0.000000000000000000, -1.000000000000000000 ) ) ;
#1713 = ORIENTED_EDGE ( 'NONE', *, *, #6768, .T. ) ;
#1714 = FACE_BOUND ( 'NONE', #7568, .T. ) ;
#1715 = CARTESIAN_POINT ( 'NONE',  ( 434.9999999999999432, -8.660254037844389075, 205.0000000000000284 ) ) ;
#1716 = CARTESIAN_POINT ( 'NONE',  ( 17.00000000000000000, 2.789133085058097101E-16, -2.055000000000000160 ) ) ;
#1717 = CARTESIAN_POINT ( 'NONE',  ( 302.6499999999999204, -75.00000000000008527, -190.0000000000000000 ) ) ;
#1718 = DIRECTION ( 'NONE',  ( -0.000000000000000000, 0.000000000000000000, -1.000000000000000000 ) ) ;
#1719 = SURFACE_STYLE_FILL_AREA ( #9641 ) ;
#1720 = AXIS2_PLACEMENT_3D ( 'NONE', #786, #10830, #13001 ) ;
#1721 = CARTESIAN_POINT ( 'NONE',  ( 302.6499999999999204, -95.00000000000008527, 169.9999999999999716 ) ) ;
#1722 = ORIENTED_EDGE ( 'NONE', *, *, #5484, .F. ) ;
#1723 = CARTESIAN_POINT ( 'NONE',  ( -299.9999999999999432, -75.00000000000008527, 354.1421356237308942 ) ) ;
#1724 = ORIENTED_EDGE ( 'NONE', *, *, #11002, .T. ) ;
#1725 = DIRECTION ( 'NONE',  ( -0.000000000000000000, -0.000000000000000000, -1.000000000000000000 ) ) ;
#1726 = DIRECTION ( 'NONE',  ( 0.000000000000000000, 0.000000000000000000, 1.000000000000000000 ) ) ;
#1727 = AXIS2_PLACEMENT_3D ( 'NONE', #10900, #5387, #9814 ) ;
#1728 = CIRCLE ( 'NONE', #7063, 5.500000000000005329 ) ;
#1729 = ORIENTED_EDGE ( 'NONE', *, *, #11443, .F. ) ;
#1730 = CARTESIAN_POINT ( 'NONE',  ( 2.500000000000000000, 0.000000000000000000, 0.000000000000000000 ) ) ;
#1731 = ORIENTED_EDGE ( 'NONE', *, *, #13950, .F. ) ;
#1732 = CARTESIAN_POINT ( 'NONE',  ( 269.0000000000000000, -8.660254037844389075, 200.0000000000000000 ) ) ;
#1733 = DIRECTION ( 'NONE',  ( -0.000000000000000000, -0.000000000000000000, -1.000000000000000000 ) ) ;
#1734 = ORIENTED_EDGE ( 'NONE', *, *, #8640, .F. ) ;
#1735 = CARTESIAN_POINT ( 'NONE',  ( 79.99999999999971578, 35.00000000000000000, 0.000000000000000000 ) ) ;
#1736 = FACE_OUTER_BOUND ( 'NONE', #10449, .T. ) ;
#1737 = EDGE_CURVE ( 'NONE', #7052, #14164, #9096, .T. ) ;
#1738 = DIRECTION ( 'NONE',  ( 0.000000000000000000, 0.000000000000000000, -1.000000000000000000 ) ) ;
#1739 = PRODUCT_CONTEXT ( 'NONE', #11106, 'mechanical' ) ;
#1740 = FACE_BOUND ( 'NONE', #8515, .T. ) ;
#1741 = VECTOR ( 'NONE', #6342, 1000.000000000000000 ) ;
#1742 = ORIENTED_EDGE ( 'NONE', *, *, #293, .T. ) ;
#1743 = ORIENTED_EDGE ( 'NONE', *, *, #2065, .T. ) ;
#1744 = ORIENTED_EDGE ( 'NONE', *, *, #2581, .T. ) ;
#1745 = ORIENTED_EDGE ( 'NONE', *, *, #4492, .F. ) ;
#1746 = CARTESIAN_POINT ( 'NONE',  ( 269.0000000000000000, 8.660254037844390851, 205.0000000000000284 ) ) ;
#1747 = ORIENTED_EDGE ( 'NONE', *, *, #5401, .T. ) ;
#1748 = DIRECTION ( 'NONE',  ( 1.000000000000000000, 0.000000000000000000, 0.000000000000000000 ) ) ;
#1749 = ORIENTED_EDGE ( 'NONE', *, *, #9790, .T. ) ;
#1750 = CARTESIAN_POINT ( 'NONE',  ( -20.63749999999999929, 1.353234713057825478E-15, 11.05000000000000071 ) ) ;
#1751 = TOROIDAL_SURFACE ( 'NONE', #9875, 13.29999999999999893, 0.2000000000000027034 ) ;
#1752 = LINE ( 'NONE', #10626, #3426 ) ;
#1753 = FACE_BOUND ( 'NONE', #3200, .T. ) ;
#1754 = AXIS2_PLACEMENT_3D ( 'NONE', #8777, #4361, #2243 ) ;
#1755 = CARTESIAN_POINT ( 'NONE',  ( -20.63749999999999574, 1.564486285910743648E-15, 12.77499999999999858 ) ) ;
#1756 = CARTESIAN_POINT ( 'NONE',  ( 140.0000000000000000, -75.00000000000008527, -186.2999999999999829 ) ) ;
#1757 = CIRCLE ( 'NONE', #14043, 2.649999999999985700 ) ;
#1758 = EDGE_LOOP ( 'NONE', ( #2832, #4777, #13936 ) ) ;
#1759 = ORIENTED_EDGE ( 'NONE', *, *, #11011, .F. ) ;
#1760 = ADVANCED_BREP_SHAPE_REPRESENTATION ( '', ( #3714, #14039 ), #3087 ) ;
#1761 = EDGE_CURVE ( 'NONE', #2628, #4723, #12763, .T. ) ;
#1763 = DIRECTION ( 'NONE',  ( 0.000000000000000000, -1.000000000000000000, 1.471414886128461471E-15 ) ) ;
#1762 = AXIS2_PLACEMENT_3D ( 'NONE', #10106, #12144, #3519 ) ;
#1764 = EDGE_CURVE ( 'NONE', #649, #298, #8332, .T. ) ;
#1765 =( REPRESENTATION_RELATIONSHIP ('NONE','NONE', #11251, #2275 ) REPRESENTATION_RELATIONSHIP_WITH_TRANSFORMATION ( #9791 )SHAPE_REPRESENTATION_RELATIONSHIP( ) );
#1766 = CARTESIAN_POINT ( 'NONE',  ( -294.9999999999999432, -65.00000000000011369, 30.00000000000000000 ) ) ;
#1767 = CYLINDRICAL_SURFACE ( 'NONE', #6316, 2.500000000000002220 ) ;
#1768 = DIRECTION ( 'NONE',  ( 1.000000000000000000, 0.000000000000000000, 0.000000000000000000 ) ) ;
#1769 = AXIS2_PLACEMENT_3D ( 'NONE', #10108, #5900, #4680 ) ;
#1770 = VERTEX_POINT ( 'NONE', #1807 ) ;
#1771 = VECTOR ( 'NONE', #2160, 1000.000000000000000 ) ;
#1772 = VECTOR ( 'NONE', #10843, 1000.000000000000000 ) ;
#1773 = FACE_BOUND ( 'NONE', #3437, .T. ) ;
#1774 = EDGE_CURVE ( 'NONE', #1625, #278, #2983, .T. ) ;
#1775 = VECTOR ( 'NONE', #12933, 1000.000000000000114 ) ;
#1776 = CARTESIAN_POINT ( 'NONE',  ( 386.6666666666666288, -20.00000000000000000, -222.5000000000000853 ) ) ;
#1777 = CARTESIAN_POINT ( 'NONE',  ( 140.0000000000000000, -75.00000000000008527, -190.0000000000000000 ) ) ;
#1778 = VECTOR ( 'NONE', #10166, 999.9999999999998863 ) ;
#1779 = LINE ( 'NONE', #8531, #7857 ) ;
#1780 = AXIS2_PLACEMENT_3D ( 'NONE', #6415, #6701, #9827 ) ;
#1781 = ORIENTED_EDGE ( 'NONE', *, *, #1695, .T. ) ;
#1782 = EDGE_CURVE ( 'NONE', #13211, #246, #5177, .T. ) ;
#1783 = DIRECTION ( 'NONE',  ( -1.000000000000000000, -0.000000000000000000, -0.000000000000000000 ) ) ;
#1784 = TOROIDAL_SURFACE ( 'NONE', #13934, 13.29999999999999893, 0.2000000000000027034 ) ;
#1785 = CARTESIAN_POINT ( 'NONE',  ( 119.9999999999999147, -20.00000000000000000, -19.99999999999998934 ) ) ;
#1786 = VECTOR ( 'NONE', #402, 1000.000000000000114 ) ;
#1787 = VECTOR ( 'NONE', #4780, 1000.000000000000000 ) ;
#1788 = EDGE_LOOP ( 'NONE', ( #3445, #8098, #4357, #6788 ) ) ;
#1789 = DIRECTION ( 'NONE',  ( -0.000000000000000000, -0.000000000000000000, 1.000000000000000000 ) ) ;
#1790 = DIRECTION ( 'NONE',  ( 0.000000000000000000, -1.000000000000000000, 0.000000000000000000 ) ) ;
#1791 = ADVANCED_FACE ( 'NONE', ( #11678 ), #8406, .T. ) ;
#1792 = ADVANCED_FACE ( 'NONE', ( #5012 ), #10742, .F. ) ;
#1793 = DIRECTION ( 'NONE',  ( 1.000000000000000000, 0.000000000000000000, 0.000000000000000000 ) ) ;
#1794 = AXIS2_PLACEMENT_3D ( 'NONE', #11740, #10875, #9715 ) ;
#1795 = CARTESIAN_POINT ( 'NONE',  ( 303.3333333333333144, -25.00000000000000000, 222.5000000000000853 ) ) ;
#1796 =( NAMED_UNIT ( * ) SI_UNIT ( $, .STERADIAN. ) SOLID_ANGLE_UNIT ( ) );
#1797 = EDGE_CURVE ( 'NONE', #2838, #12140, #769, .T. ) ;
#1798 = EDGE_CURVE ( 'NONE', #6723, #8744, #10669, .T. ) ;
#1799 = CARTESIAN_POINT ( 'NONE',  ( -0.5276280594146446346, 4.314175951381965746, -3.320322319201721495 ) ) ;
#1800 = ITEM_DEFINED_TRANSFORMATION ( 'NONE', 'NONE', #11179,  #14039 ) ;
#1801 = CIRCLE ( 'NONE', #13382, 2.649999999999985700 ) ;
#1802 = EDGE_LOOP ( 'NONE', ( #7587, #12705 ) ) ;
#1803 = EDGE_CURVE ( 'NONE', #11373, #11952, #13987, .T. ) ;
#1804 = FACE_OUTER_BOUND ( 'NONE', #8996, .T. ) ;
#1805 = EDGE_LOOP ( 'NONE', ( #3227, #10313 ) ) ;
#1806 = CARTESIAN_POINT ( 'NONE',  ( -297.4999999999999432, -75.00000000000008527, 0.000000000000000000 ) ) ;
#1807 = CARTESIAN_POINT ( 'NONE',  ( -5.000000000000000888, 8.660254037844387298, -200.0000000000000000 ) ) ;
#1808 = VERTEX_POINT ( 'NONE', #13773 ) ;
#1809 = DIRECTION ( 'NONE',  ( -1.000000000000000000, 0.000000000000000000, 0.000000000000000000 ) ) ;
#1810 = VERTEX_POINT ( 'NONE', #2905 ) ;
#1811 = LINE ( 'NONE', #9801, #6630 ) ;
#1812 = CARTESIAN_POINT ( 'NONE',  ( 0.000000000000000000, 0.000000000000000000, 0.000000000000000000 ) ) ;
#1813 = ORIENTED_EDGE ( 'NONE', *, *, #10581, .F. ) ;
#1814 =( NAMED_UNIT ( * ) PLANE_ANGLE_UNIT ( ) SI_UNIT ( $, .RADIAN. ) );
#1815 = CIRCLE ( 'NONE', #893, 2.500000000000002220 ) ;
#1816 = DIRECTION ( 'NONE',  ( 0.000000000000000000, 0.000000000000000000, 1.000000000000000000 ) ) ;
#1817 = SURFACE_STYLE_USAGE ( .BOTH. , #14141 ) ;
#1818 = DIRECTION ( 'NONE',  ( 1.000000000000000000, 9.912705577010325549E-17, 0.000000000000000000 ) ) ;
#1819 = ITEM_DEFINED_TRANSFORMATION ( 'NONE', 'NONE', #11634,  #14039 ) ;
#1820 = DIRECTION ( 'NONE',  ( 1.000000000000000000, 0.000000000000000000, 0.000000000000000000 ) ) ;
#1821 = EDGE_LOOP ( 'NONE', ( #3567, #69 ) ) ;
#1822 = EDGE_LOOP ( 'NONE', ( #13493, #1021, #5094, #2101 ) ) ;
#1823 = AXIS2_PLACEMENT_3D ( 'NONE', #9966, #8876, #203 ) ;
#1824 = ORIENTED_EDGE ( 'NONE', *, *, #4456, .T. ) ;
#1825 = ORIENTED_EDGE ( 'NONE', *, *, #5920, .F. ) ;
#1826 = DIRECTION ( 'NONE',  ( 0.8571673013836870192, 0.000000000000000000, 0.5150380737757234151 ) ) ;
#1827 = EDGE_CURVE ( 'NONE', #2165, #7848, #10425, .T. ) ;
#1828 = ORIENTED_EDGE ( 'NONE', *, *, #9026, .F. ) ;
#1829 = LINE ( 'NONE', #793, #10825 ) ;
#1830 = ORIENTED_EDGE ( 'NONE', *, *, #13625, .T. ) ;
#1831 = DIRECTION ( 'NONE',  ( -1.000000000000000000, -2.478176394252579230E-17, -0.000000000000000000 ) ) ;
#1832 = DIRECTION ( 'NONE',  ( -1.000000000000000000, 0.000000000000000000, 0.000000000000000000 ) ) ;
#1833 = LINE ( 'NONE', #578, #3409 ) ;
#1834 = DIRECTION ( 'NONE',  ( 0.000000000000000000, 1.000000000000000000, 0.000000000000000000 ) ) ;
#1835 = LINE ( 'NONE', #8586, #5136 ) ;
#1836 = CIRCLE ( 'NONE', #13404, 10.00000000000000000 ) ;
#1837 = PLANE ( 'NONE',  #4145 ) ;
#1838 = PRODUCT_DEFINITION_SHAPE ( 'NONE', 'NONE',  #14359 ) ;
#1839 = VERTEX_POINT ( 'NONE', #7173 ) ;
#1840 = CIRCLE ( 'NONE', #3596, 0.8509999999999999787 ) ;
#1841 = ORIENTED_EDGE ( 'NONE', *, *, #3449, .T. ) ;
#1842 = FACE_OUTER_BOUND ( 'NONE', #7097, .T. ) ;
#1843 = EDGE_CURVE ( 'NONE', #915, #2687, #631, .T. ) ;
#1844 = ORIENTED_EDGE ( 'NONE', *, *, #1574, .T. ) ;
#1845 = CARTESIAN_POINT ( 'NONE',  ( 434.9999999999999432, -8.660254037844389075, 200.0000000000000000 ) ) ;
#1846 = TOROIDAL_SURFACE ( 'NONE', #3702, 11.75000000000000000, 1.050000000000000266 ) ;
#1847 = FACE_OUTER_BOUND ( 'NONE', #5801, .T. ) ;
#1848 =( LENGTH_UNIT ( ) NAMED_UNIT ( * ) SI_UNIT ( .MILLI., .METRE. ) );
#1849 = AXIS2_PLACEMENT_3D ( 'NONE', #7156, #3900, #4772 ) ;
#1850 = VERTEX_POINT ( 'NONE', #7316 ) ;
#1851 = VECTOR ( 'NONE', #10499, 1000.000000000000000 ) ;
#1852 = CIRCLE ( 'NONE', #9540, 13.50000000000000533 ) ;
#1853 = DIRECTION ( 'NONE',  ( 0.000000000000000000, -1.000000000000000000, 1.287488025362403787E-15 ) ) ;
#1854 = EDGE_CURVE ( 'NONE', #8482, #10176, #4060, .T. ) ;
#1855 = FACE_OUTER_BOUND ( 'NONE', #9978, .T. ) ;
#1856 = DIRECTION ( 'NONE',  ( -1.000000000000000000, 0.000000000000000000, 0.000000000000000000 ) ) ;
#1857 = DIRECTION ( 'NONE',  ( -1.000000000000000000, 0.000000000000000000, 0.000000000000000000 ) ) ;
#1858 = ORIENTED_EDGE ( 'NONE', *, *, #728, .F. ) ;
#1859 = ORIENTED_EDGE ( 'NONE', *, *, #5608, .F. ) ;
#1860 = DIRECTION ( 'NONE',  ( 0.000000000000000000, 0.000000000000000000, 1.000000000000000000 ) ) ;
#1861 = AXIS2_PLACEMENT_3D ( 'NONE', #3908, #10435, #11668 ) ;
#1862 = FACE_BOUND ( 'NONE', #627, .T. ) ;
#1863 = ORIENTED_EDGE ( 'NONE', *, *, #9958, .T. ) ;
#1864 = DIRECTION ( 'NONE',  ( 0.000000000000000000, 0.000000000000000000, 1.000000000000000000 ) ) ;
#1865 =( NAMED_UNIT ( * ) SI_UNIT ( $, .STERADIAN. ) SOLID_ANGLE_UNIT ( ) );
#1866 = VECTOR ( 'NONE', #11220, 1000.000000000000000 ) ;
#1867 =( NAMED_UNIT ( * ) PLANE_ANGLE_UNIT ( ) SI_UNIT ( $, .RADIAN. ) );
#1868 = EDGE_CURVE ( 'NONE', #5579, #9676, #6023, .T. ) ;
#1869 = CARTESIAN_POINT ( 'NONE',  ( 4.000000000000000000, -2.511475576507276042, -3.469253905236643565 ) ) ;
#1870 = PRODUCT_DEFINITION ( 'UNKNOWN', '', #8642, #2767 ) ;
#1871 = DIRECTION ( 'NONE',  ( -0.000000000000000000, -0.000000000000000000, -1.000000000000000000 ) ) ;
#1872 = VERTEX_POINT ( 'NONE', #11824 ) ;
#1873 = CARTESIAN_POINT ( 'NONE',  ( 93.00000000000000000, 8.660254037844390851, 199.9990000000000236 ) ) ;
#1874 = AXIS2_PLACEMENT_3D ( 'NONE', #7138, #430, #13658 ) ;
#1875 = ORIENTED_EDGE ( 'NONE', *, *, #7549, .T. ) ;
#1876 = CARTESIAN_POINT ( 'NONE',  ( 305.4999999999999432, -75.00000000000008527, 186.2999999999999829 ) ) ;
#1877 = DIRECTION ( 'NONE',  ( -0.000000000000000000, 0.000000000000000000, -1.000000000000000000 ) ) ;
#1878 = EDGE_CURVE ( 'NONE', #13081, #11113, #4181, .T. ) ;
#1879 = ADVANCED_FACE ( 'NONE', ( #10446 ), #1655, .F. ) ;
#1880 = EDGE_CURVE ( 'NONE', #1400, #5301, #9434, .T. ) ;
#1881 = VERTEX_POINT ( 'NONE', #5371 ) ;
#1882 = EDGE_CURVE ( 'NONE', #10615, #4007, #6455, .T. ) ;
#1883 = CARTESIAN_POINT ( 'NONE',  ( -4.211140560182196957, 2.431303136016537803, -3.745885042887433514 ) ) ;
#1884 = ORIENTED_EDGE ( 'NONE', *, *, #9683, .T. ) ;
#1885 =( GEOMETRIC_REPRESENTATION_CONTEXT ( 3 ) GLOBAL_UNCERTAINTY_ASSIGNED_CONTEXT ( ( #10697 ) ) GLOBAL_UNIT_ASSIGNED_CONTEXT ( ( #659, #9826, #6700 ) ) REPRESENTATION_CONTEXT ( 'NONE', 'WORKASPACE' ) );
#1886 = DIRECTION ( 'NONE',  ( -0.000000000000000000, -0.000000000000000000, 1.000000000000000000 ) ) ;
#1887 = CARTESIAN_POINT ( 'NONE',  ( -219.9999999999999147, -85.00000000000009948, 30.00000000000000000 ) ) ;
#1888 = EDGE_LOOP ( 'NONE', ( #4304, #13023 ) ) ;
#1889 = DIRECTION ( 'NONE',  ( 1.000000000000000000, 0.000000000000000000, 0.000000000000000000 ) ) ;
#1890 = DIRECTION ( 'NONE',  ( -1.000000000000000000, -0.000000000000000000, -0.000000000000000000 ) ) ;
#1891 =( LENGTH_UNIT ( ) NAMED_UNIT ( * ) SI_UNIT ( .MILLI., .METRE. ) );
#1892 = VECTOR ( 'NONE', #2249, 1000.000000000000000 ) ;
#1893 = CONTEXT_DEPENDENT_SHAPE_REPRESENTATION ( #11755, #13633 ) ;
#1894 = DIRECTION ( 'NONE',  ( 0.000000000000000000, -1.000000000000000000, 0.000000000000000000 ) ) ;
#1895 =( GEOMETRIC_REPRESENTATION_CONTEXT ( 3 ) GLOBAL_UNCERTAINTY_ASSIGNED_CONTEXT ( ( #757 ) ) GLOBAL_UNIT_ASSIGNED_CONTEXT ( ( #6447, #10585, #1796 ) ) REPRESENTATION_CONTEXT ( 'NONE', 'WORKASPACE' ) );
#1896 = VERTEX_POINT ( 'NONE', #14270 ) ;
#1897 = EDGE_CURVE ( 'NONE', #532, #10192, #9273, .T. ) ;
#1898 = EDGE_LOOP ( 'NONE', ( #8131, #4401, #5922 ) ) ;
#1899 = FACE_OUTER_BOUND ( 'NONE', #4056, .T. ) ;
#1900 = VERTEX_POINT ( 'NONE', #986 ) ;
#1901 = CARTESIAN_POINT ( 'NONE',  ( 1.794155980045911036, 0.000000000000000000, 0.000000000000000000 ) ) ;
#1902 = ORIENTED_EDGE ( 'NONE', *, *, #14091, .T. ) ;
#1903 = CIRCLE ( 'NONE', #2841, 0.2500000000000002220 ) ;
#1904 = VERTEX_POINT ( 'NONE', #5305 ) ;
#1905 = DIRECTION ( 'NONE',  ( -0.3090169943749412895, 0.000000000000000000, 0.9510565162951555296 ) ) ;
#1906 = ORIENTED_EDGE ( 'NONE', *, *, #6410, .T. ) ;
#1907 = CARTESIAN_POINT ( 'NONE',  ( -1.799999999999996048, 0.000000000000000000, 0.000000000000000000 ) ) ;
#1908 = AXIS2_PLACEMENT_3D ( 'NONE', #10790, #13892, #8453 ) ;
#1909 = CARTESIAN_POINT ( 'NONE',  ( -30.00000000000002842, -20.00000000000000000, 200.0000000000000000 ) ) ;
#1910 = LINE ( 'NONE', #1013, #138 ) ;
#1911 = CIRCLE ( 'NONE', #9558, 2.649999999999985700 ) ;
#1912 = UNCERTAINTY_MEASURE_WITH_UNIT (LENGTH_MEASURE( 1.000000000000000082E-05 ), #12564, 'distance_accuracy_value', 'NONE');
#1913 = LINE ( 'NONE', #1755, #1633 ) ;
#1914 = CARTESIAN_POINT ( 'NONE',  ( 2.740000000000000213, 0.9838866223910001096, -0.5150000000000001243 ) ) ;
#1915 = CIRCLE ( 'NONE', #2620, 0.2000000000000000944 ) ;
#1916 = ORIENTED_EDGE ( 'NONE', *, *, #4025, .F. ) ;
#1917 = EDGE_CURVE ( 'NONE', #7052, #10809, #14121, .T. ) ;
#1918 = VERTEX_POINT ( 'NONE', #12111 ) ;
#1919 = CARTESIAN_POINT ( 'NONE',  ( 132.3499999999999943, 45.00000000000001421, 0.000000000000000000 ) ) ;
#1920 = CARTESIAN_POINT ( 'NONE',  ( -30.00000000000002842, -225.0000000000000000, 190.0000000000000000 ) ) ;
#1921 = CARTESIAN_POINT ( 'NONE',  ( 136.6666666666666288, -20.00000000000000000, 225.1500000000000625 ) ) ;
#1922 = AXIS2_PLACEMENT_3D ( 'NONE', #7315, #6093, #11752 ) ;
#1923 = PRESENTATION_STYLE_ASSIGNMENT (( #12732 ) ) ;
#1924 = APPLICATION_CONTEXT ( 'automotive_design' ) ;
#1925 = ORIENTED_EDGE ( 'NONE', *, *, #12785, .F. ) ;
#1926 = CARTESIAN_POINT ( 'NONE',  ( 299.9999999999999432, -75.00000000000008527, 190.0000000000000000 ) ) ;
#1927 = LINE ( 'NONE', #5283, #4858 ) ;
#1928 = CARTESIAN_POINT ( 'NONE',  ( 0.000000000000000000, -20.00000000000000000, 169.9999999999999716 ) ) ;
#1929 = CARTESIAN_POINT ( 'NONE',  ( 134.9999999999999432, -36.99999999999997868, 0.000000000000000000 ) ) ;
#1930 = ADVANCED_FACE ( 'NONE', ( #8772 ), #14063, .F. ) ;
#1931 = EDGE_LOOP ( 'NONE', ( #1371, #6287 ) ) ;
#1932 = ORIENTED_EDGE ( 'NONE', *, *, #10342, .F. ) ;
#1933 = DIRECTION ( 'NONE',  ( 1.000000000000000000, 0.000000000000000000, 0.000000000000000000 ) ) ;
#1934 = DIRECTION ( 'NONE',  ( 0.000000000000000000, 0.000000000000000000, -1.000000000000000000 ) ) ;
#1935 = ADVANCED_FACE ( 'NONE', ( #908 ), #6526, .F. ) ;
#1936 = EDGE_LOOP ( 'NONE', ( #2189, #10105 ) ) ;
#1937 = DIRECTION ( 'NONE',  ( 0.000000000000000000, -0.4999999999999993894, 0.8660254037844389297 ) ) ;
#1938 = PLANE ( 'NONE',  #1794 ) ;
#1939 = DIRECTION ( 'NONE',  ( -1.000000000000000000, 0.000000000000000000, -0.000000000000000000 ) ) ;
#1940 = DIRECTION ( 'NONE',  ( -0.000000000000000000, 0.000000000000000000, -1.000000000000000000 ) ) ;
#1941 =( NAMED_UNIT ( * ) PLANE_ANGLE_UNIT ( ) SI_UNIT ( $, .RADIAN. ) );
#1942 = ORIENTED_EDGE ( 'NONE', *, *, #7387, .F. ) ;
#1943 = DIRECTION ( 'NONE',  ( -0.000000000000000000, 0.8660254037844390407, 0.4999999999999993339 ) ) ;
#1944 = ORIENTED_EDGE ( 'NONE', *, *, #5173, .F. ) ;
#1945 = CARTESIAN_POINT ( 'NONE',  ( -30.00000000000002842, -225.0000000000000000, -190.0000000000000000 ) ) ;
#1946 = CARTESIAN_POINT ( 'NONE',  ( -31.74999999999995737, 0.000000000000000000, 4.250000000000000000 ) ) ;
#1947 = EDGE_CURVE ( 'NONE', #6913, #4174, #10811, .T. ) ;
#1948 = EDGE_CURVE ( 'NONE', #3491, #8933, #13191, .T. ) ;
#1949 = ORIENTED_EDGE ( 'NONE', *, *, #11119, .T. ) ;
#1950 = CARTESIAN_POINT ( 'NONE',  ( 0.000000000000000000, 2.357898499370431722, -2.818925648462311528E-15 ) ) ;
#1951 = ORIENTED_EDGE ( 'NONE', *, *, #14113, .T. ) ;
#1952 = CARTESIAN_POINT ( 'NONE',  ( 170.9999999999999716, 8.660254037844390851, 199.9990000000000236 ) ) ;
#1953 = PRODUCT_DEFINITION_SHAPE ( 'NONE', 'NONE',  #14381 ) ;
#1954 = CARTESIAN_POINT ( 'NONE',  ( -4.197393957002303999, -0.8151795401431414234, -3.503767560748935139 ) ) ;
#1955 = ORIENTED_EDGE ( 'NONE', *, *, #9788, .F. ) ;
#1956 = CARTESIAN_POINT ( 'NONE',  ( 7.345657149124969365, -5.313980200056029618E-16, -1.312408941149200148 ) ) ;
#1957 = DIRECTION ( 'NONE',  ( 1.000000000000000000, 0.000000000000000000, 0.000000000000000000 ) ) ;
#1958 =( NAMED_UNIT ( * ) PLANE_ANGLE_UNIT ( ) SI_UNIT ( $, .RADIAN. ) );
#1959 = DIRECTION ( 'NONE',  ( 0.000000000000000000, 0.8660254037844380415, -0.5000000000000009992 ) ) ;
#1960 = CONTEXT_DEPENDENT_SHAPE_REPRESENTATION ( #11016, #9931 ) ;
#1961 = ADVANCED_FACE ( 'NONE', ( #4276 ), #8696, .F. ) ;
#1962 = CARTESIAN_POINT ( 'NONE',  ( -4.000000000000000000, 1.677772373332757194, -3.535253723897187506 ) ) ;
#1963 = ORIENTED_EDGE ( 'NONE', *, *, #5243, .F. ) ;
#1964 = VERTEX_POINT ( 'NONE', #2095 ) ;
#1965 = CARTESIAN_POINT ( 'NONE',  ( -124.9999999999999432, 55.00000000000001421, 40.00000000000000000 ) ) ;
#1966 = VECTOR ( 'NONE', #6891, 1000.000000000000000 ) ;
#1967 = CIRCLE ( 'NONE', #2433, 2.041999999999999815 ) ;
#1968 = ORIENTED_EDGE ( 'NONE', *, *, #13609, .F. ) ;
#1969 = CARTESIAN_POINT ( 'NONE',  ( -4.101948962586059011, 2.368261337751163875, -3.681124513963739187 ) ) ;
#1970 = EDGE_CURVE ( 'NONE', #11219, #6474, #3127, .T. ) ;
#1971 = VERTEX_POINT ( 'NONE', #11900 ) ;
#1972 = ORIENTED_EDGE ( 'NONE', *, *, #8819, .T. ) ;
#1973 = DIRECTION ( 'NONE',  ( -1.000000000000000000, -7.304098846218135653E-17, 0.000000000000000000 ) ) ;
#1974 = ORIENTED_EDGE ( 'NONE', *, *, #10486, .F. ) ;
#1975 = DIRECTION ( 'NONE',  ( -0.000000000000000000, 0.000000000000000000, -1.000000000000000000 ) ) ;
#1976 = CARTESIAN_POINT ( 'NONE',  ( 0.000000000000000000, 0.000000000000000000, 200.0000000000000000 ) ) ;
#1977 = DIRECTION ( 'NONE',  ( 1.000000000000000000, 0.000000000000000000, 0.000000000000000000 ) ) ;
#1978 = AXIS2_PLACEMENT_3D ( 'NONE', #6016, #10442, #475 ) ;
#1979 = CARTESIAN_POINT ( 'NONE',  ( 12.00000000000000000, 1.469576158976823947E-15, 186.0000000000000000 ) ) ;
#1980 = ADVANCED_FACE ( 'NONE', ( #3271 ), #7602, .F. ) ;
#1981 = FACE_BOUND ( 'NONE', #1821, .T. ) ;
#1982 = VERTEX_POINT ( 'NONE', #12040 ) ;
#1983 = ADVANCED_FACE ( 'NONE', ( #2021 ), #7673, .T. ) ;
#1984 = VERTEX_POINT ( 'NONE', #5506 ) ;
#1985 = B_SPLINE_CURVE_WITH_KNOTS ( 'NONE', 3,
 ( #6018, #6839, #213, #478, #3054, #7394 ),
 .UNSPECIFIED., .F., .F.,
 ( 4, 2, 4 ),
 ( -3.640115492407174633E-06, 0.0002066546034003413743, 0.0004169493222930899571 ),
 .UNSPECIFIED. ) ;
#1986 = ADVANCED_FACE ( 'NONE', ( #9934 ), #5229, .F. ) ;
#1987 = FACE_OUTER_BOUND ( 'NONE', #13855, .T. ) ;
#1988 = VECTOR ( 'NONE', #8190, 1000.000000000000000 ) ;
#1989 = ORIENTED_EDGE ( 'NONE', *, *, #10530, .F. ) ;
#1990 = CARTESIAN_POINT ( 'NONE',  ( 303.3333333333333144, -20.00000000000000000, 222.5000000000000853 ) ) ;
#1991 = CARTESIAN_POINT ( 'NONE',  ( 2.805705207896068476, -3.226868319750173075, -3.503898532754370354 ) ) ;
#1992 = ORIENTED_EDGE ( 'NONE', *, *, #5529, .T. ) ;
#1993 = FACE_BOUND ( 'NONE', #863, .T. ) ;
#1994 = AXIS2_PLACEMENT_3D ( 'NONE', #3763, #10431, #6004 ) ;
#1995 = CARTESIAN_POINT ( 'NONE',  ( -30.00000000000002842, -25.00000000000000000, 169.9999999999999716 ) ) ;
#1996 = APPLICATION_PROTOCOL_DEFINITION ( 'draft international standard', 'automotive_design', 1998, #4616 ) ;
#1997 = DIRECTION ( 'NONE',  ( -1.000000000000000000, 0.000000000000000000, 0.000000000000000000 ) ) ;
#1998 = CIRCLE ( 'NONE', #11968, 10.00000000000000000 ) ;
#1999 = ORIENTED_EDGE ( 'NONE', *, *, #7259, .T. ) ;
#2000 = EDGE_LOOP ( 'NONE', ( #1745, #12037, #3225, #9323 ) ) ;
#2001 = CYLINDRICAL_SURFACE ( 'NONE', #4420, 2.500000000000000444 ) ;
#2002 = LINE ( 'NONE', #6441, #9050 ) ;
#2003 = CIRCLE ( 'NONE', #14082, 2.649999999999985700 ) ;
#2004 = VECTOR ( 'NONE', #287, 1000.000000000000000 ) ;
#2005 = EDGE_CURVE ( 'NONE', #8555, #11820, #8573, .T. ) ;
#2006 = VERTEX_POINT ( 'NONE', #10647 ) ;
#2007 = PLANE ( 'NONE',  #6419 ) ;
#2008 = VECTOR ( 'NONE', #8358, 1000.000000000000000 ) ;
#2009 = CARTESIAN_POINT ( 'NONE',  ( -2.500000000000000444, 3.061616997868383634E-16, -5.000000000000000888 ) ) ;
#2010 = FACE_OUTER_BOUND ( 'NONE', #1073, .T. ) ;
#2011 = FILL_AREA_STYLE ('',( #623 ) ) ;
#2012 = VECTOR ( 'NONE', #9533, 999.9999999999997726 ) ;
#2013 = ITEM_DEFINED_TRANSFORMATION ( 'NONE', 'NONE', #4690,  #14039 ) ;
#2014 = MECHANICAL_DESIGN_GEOMETRIC_PRESENTATION_REPRESENTATION (  '', ( #1314 ), #4345 ) ;
#2015 = ORIENTED_EDGE ( 'NONE', *, *, #9683, .F. ) ;
#2016 = CIRCLE ( 'NONE', #4589, 2.649999999999985700 ) ;
#2017 = CARTESIAN_POINT ( 'NONE',  ( -307.6499999999999204, 45.00000000000001421, 40.00000000000000000 ) ) ;
#2018 = CIRCLE ( 'NONE', #3199, 5.500000000000005329 ) ;
#2019 = VERTEX_POINT ( 'NONE', #818 ) ;
#2020 = DIRECTION ( 'NONE',  ( 0.8571673013836870192, 0.000000000000000000, 0.5150380737757234151 ) ) ;
#2021 = FACE_OUTER_BOUND ( 'NONE', #12943, .T. ) ;
#2022 = EDGE_CURVE ( 'NONE', #11916, #14253, #9557, .T. ) ;
#2023 = CIRCLE ( 'NONE', #1075, 2.649999999999985700 ) ;
#2024 = EDGE_LOOP ( 'NONE', ( #7453, #13722, #2432, #3268 ) ) ;
#2025 = EDGE_LOOP ( 'NONE', ( #10502, #12176, #5270, #9510 ) ) ;
#2026 = DIRECTION ( 'NONE',  ( -0.000000000000000000, -0.000000000000000000, -1.000000000000000000 ) ) ;
#2027 = AXIS2_PLACEMENT_3D ( 'NONE', #10148, #6674, #12325 ) ;
#2028 = CARTESIAN_POINT ( 'NONE',  ( 307.5000000000000000, -36.99999999999997868, -169.9999999999999716 ) ) ;
#2029 = ORIENTED_EDGE ( 'NONE', *, *, #10050, .T. ) ;
#2030 = CIRCLE ( 'NONE', #5739, 2.500000000000002220 ) ;
#2031 = CARTESIAN_POINT ( 'NONE',  ( 2.740000000000000213, -0.5150000000000022338, 0.6774776749089210792 ) ) ;
#2032 = CARTESIAN_POINT ( 'NONE',  ( 5.000000000000000888, 4.250000000000000000, 0.000000000000000000 ) ) ;
#2033 = ADVANCED_FACE ( 'NONE', ( #9479 ), #9743, .F. ) ;
#2034 = CARTESIAN_POINT ( 'NONE',  ( 2.500000000000000000, -1.178949249685213863, 2.042000000000002924 ) ) ;
#2035 = EDGE_CURVE ( 'NONE', #10043, #13274, #4113, .T. ) ;
#2036 = VERTEX_POINT ( 'NONE', #3816 ) ;
#2037 = ORIENTED_EDGE ( 'NONE', *, *, #1146, .T. ) ;
#2038 = CARTESIAN_POINT ( 'NONE',  ( 3.699999999999998401, 0.000000000000000000, 4.750000000000000000 ) ) ;
#2039 = ORIENTED_EDGE ( 'NONE', *, *, #8435, .T. ) ;
#2040 = DIRECTION ( 'NONE',  ( -0.000000000000000000, 1.000000000000000000, 0.000000000000000000 ) ) ;
#2041 = UNCERTAINTY_MEASURE_WITH_UNIT (LENGTH_MEASURE( 1.000000000000000082E-05 ), #8000, 'distance_accuracy_value', 'NONE');
#2042 = ORIENTED_EDGE ( 'NONE', *, *, #13545, .F. ) ;
#2043 = AXIS2_PLACEMENT_3D ( 'NONE', #5978, #13653, #10473 ) ;
#2044 = ORIENTED_EDGE ( 'NONE', *, *, #7068, .F. ) ;
#2045 = DIRECTION ( 'NONE',  ( -0.000000000000000000, -0.000000000000000000, 1.000000000000000000 ) ) ;
#2046 = EDGE_LOOP ( 'NONE', ( #10992, #11416, #13574, #13696 ) ) ;
#2047 = CARTESIAN_POINT ( 'NONE',  ( 170.9999999999999716, 8.660254037844390851, 200.0000000000000000 ) ) ;
#2048 = DIRECTION ( 'NONE',  ( 1.000000000000000000, 0.000000000000000000, 0.000000000000000000 ) ) ;
#2049 = CARTESIAN_POINT ( 'NONE',  ( 2.740000000000000213, -0.9838866223905674557, -0.5150000000000000133 ) ) ;
#2050 = CARTESIAN_POINT ( 'NONE',  ( 219.9999999999999147, -85.00000000000009948, -17.55500000000000327 ) ) ;
#2051 =( REPRESENTATION_RELATIONSHIP ('NONE','NONE', #11251, #208 ) REPRESENTATION_RELATIONSHIP_WITH_TRANSFORMATION ( #5725 )SHAPE_REPRESENTATION_RELATIONSHIP( ) );
#2052 = CARTESIAN_POINT ( 'NONE',  ( 200.8500000000000227, -85.00000000000007105, 50.00000000000001421 ) ) ;
#2054 = EDGE_CURVE ( 'NONE', #13344, #10688, #7295, .T. ) ;
#2053 = CIRCLE ( 'NONE', #6478, 5.500000000000005329 ) ;
#2055 = EDGE_CURVE ( 'NONE', #11403, #13651, #6360, .T. ) ;
#2056 = DIRECTION ( 'NONE',  ( 0.000000000000000000, 0.000000000000000000, 1.000000000000000000 ) ) ;
#2057 = EDGE_LOOP ( 'NONE', ( #2612, #13253 ) ) ;
#2058 = AXIS2_PLACEMENT_3D ( 'NONE', #7166, #13910, #8326 ) ;
#2059 = EDGE_LOOP ( 'NONE', ( #13294, #3495, #8438, #8654 ) ) ;
#2060 = LINE ( 'NONE', #6629, #1445 ) ;
#2061 = AXIS2_PLACEMENT_3D ( 'NONE', #5443, #1215, #5612 ) ;
#2062 = ORIENTED_EDGE ( 'NONE', *, *, #1427, .F. ) ;
#2063 = CYLINDRICAL_SURFACE ( 'NONE', #8959, 13.50000000000000000 ) ;
#2064 = CARTESIAN_POINT ( 'NONE',  ( -294.9999999999999432, -65.00000000000011369, 40.00000000000000000 ) ) ;
#2065 = EDGE_CURVE ( 'NONE', #3349, #6820, #11583, .T. ) ;
#2066 = ADVANCED_FACE ( 'NONE', ( #3968 ), #4040, .F. ) ;
#2067 = CARTESIAN_POINT ( 'NONE',  ( 119.9999999999999147, -20.00000000000000000, -169.9999999999999716 ) ) ;
#2068 = ORIENTED_EDGE ( 'NONE', *, *, #3577, .F. ) ;
#2069 = EDGE_CURVE ( 'NONE', #8138, #8017, #7226, .T. ) ;
#2070 = CIRCLE ( 'NONE', #12034, 13.50000000000000000 ) ;
#2071 = B_SPLINE_CURVE_WITH_KNOTS ( 'NONE', 3,
 ( #9165, #4753, #8906, #4416, #12235, #14257, #8832, #5565 ),
 .UNSPECIFIED., .F., .F.,
 ( 4, 2, 2, 4 ),
 ( 2.465131517075058656E-07, 0.001183067374689851080, 0.001774477805458923299, 0.002365888236227995517 ),
 .UNSPECIFIED. ) ;
#2072 = DIRECTION ( 'NONE',  ( -1.000000000000000000, 0.000000000000000000, 0.000000000000000000 ) ) ;
#2073 = CARTESIAN_POINT ( 'NONE',  ( -1.999999999999998224, 1.353234713057825478E-15, 11.05000000000000071 ) ) ;
#2074 = CARTESIAN_POINT ( 'NONE',  ( -299.9999999999999432, -75.00000000000008527, 339.9999999999999432 ) ) ;
#2075 = ORIENTED_EDGE ( 'NONE', *, *, #12736, .F. ) ;
#2076 = ORIENTED_EDGE ( 'NONE', *, *, #10879, .T. ) ;
#2077 = VECTOR ( 'NONE', #14177, 1000.000000000000000 ) ;
#2078 = DIRECTION ( 'NONE',  ( -1.000000000000000000, -0.000000000000000000, -0.000000000000000000 ) ) ;
#2079 = PRODUCT_DEFINITION_SHAPE ( 'NONE', 'NONE',  #14365 ) ;
#2080 = FACE_OUTER_BOUND ( 'NONE', #3791, .T. ) ;
#2081 = AXIS2_PLACEMENT_3D ( 'NONE', #6577, #11081, #6714 ) ;
#2082 = EDGE_LOOP ( 'NONE', ( #4217, #8427 ) ) ;
#2083 = FACE_OUTER_BOUND ( 'NONE', #13848, .T. ) ;
#2084 = DIRECTION ( 'NONE',  ( 1.000000000000000000, 0.000000000000000000, 0.000000000000000000 ) ) ;
#2085 = CARTESIAN_POINT ( 'NONE',  ( 5.000000000000004441, 0.000000000000000000, 4.250000000000000000 ) ) ;
#2086 = DIRECTION ( 'NONE',  ( -1.000000000000000000, 0.000000000000000000, 0.000000000000000000 ) ) ;
#2087 = AXIS2_PLACEMENT_3D ( 'NONE', #5034, #8498, #4079 ) ;
#2088 = ITEM_DEFINED_TRANSFORMATION ( 'NONE', 'NONE', #7919,  #14039 ) ;
#2089 = EDGE_CURVE ( 'NONE', #6981, #8456, #1779, .T. ) ;
#2090 = CONICAL_SURFACE ( 'NONE', #10199, 2.041999999999999815, 1.047197551196591858 ) ;
#2091 = ORIENTED_EDGE ( 'NONE', *, *, #3400, .T. ) ;
#2092 = DIRECTION ( 'NONE',  ( -1.000000000000000000, 0.000000000000000000, 0.000000000000000000 ) ) ;
#2093 = ORIENTED_EDGE ( 'NONE', *, *, #14011, .T. ) ;
#2094 = FACE_OUTER_BOUND ( 'NONE', #692, .T. ) ;
#2095 = CARTESIAN_POINT ( 'NONE',  ( -2.100000000000000089, 2.571758278209441957E-16, -0.2800830152838844622 ) ) ;
#2096 = VECTOR ( 'NONE', #7672, 1000.000000000000000 ) ;
#2097 = EDGE_LOOP ( 'NONE', ( #12891, #12875, #7619, #9143 ) ) ;
#2098 = EDGE_LOOP ( 'NONE', ( #8207, #7792 ) ) ;
#2099 = FACE_OUTER_BOUND ( 'NONE', #5985, .T. ) ;
#2100 = DIRECTION ( 'NONE',  ( 0.000000000000000000, 1.224646799147353207E-16, 1.000000000000000000 ) ) ;
#2101 = ORIENTED_EDGE ( 'NONE', *, *, #4096, .F. ) ;
#2102 = DIRECTION ( 'NONE',  ( 0.4461977533474923430, -0.8949343913984144638, 0.000000000000000000 ) ) ;
#2103 = COLOUR_RGB ( '',1.000000000000000000, 0.9490196078431372140, 0.9098039215686274384 ) ;
#2104 = CARTESIAN_POINT ( 'NONE',  ( 1.849560077140107950, -0.5150000000000023448, 0.7556913915602430087 ) ) ;
#2105 = DIRECTION ( 'NONE',  ( 0.000000000000000000, 0.000000000000000000, 1.000000000000000000 ) ) ;
#2106 = CARTESIAN_POINT ( 'NONE',  ( 469.9999999999998863, -225.0000000000000000, 190.0000000000000000 ) ) ;
#2107 = DIRECTION ( 'NONE',  ( 0.000000000000000000, 0.000000000000000000, 1.000000000000000000 ) ) ;
#2108 = ITEM_DEFINED_TRANSFORMATION ( 'NONE', 'NONE', #10472,  #14039 ) ;
#2109 = CARTESIAN_POINT ( 'NONE',  ( 140.0000000000000000, -75.00000000000008527, -169.9999999999999716 ) ) ;
#2110 = CIRCLE ( 'NONE', #3967, 10.20000000000000107 ) ;
#2111 = EDGE_LOOP ( 'NONE', ( #2285, #9909, #3142, #4212 ) ) ;
#2112 = ORIENTED_EDGE ( 'NONE', *, *, #1524, .F. ) ;
#2113 = FACE_OUTER_BOUND ( 'NONE', #6177, .T. ) ;
#2114 = APPLICATION_CONTEXT ( 'automotive_design' ) ;
#2115 = ORIENTED_EDGE ( 'NONE', *, *, #12561, .F. ) ;
#2116 = VECTOR ( 'NONE', #855, 1000.000000000000000 ) ;
#2117 = FACE_OUTER_BOUND ( 'NONE', #11878, .T. ) ;
#2118 = ORIENTED_EDGE ( 'NONE', *, *, #10938, .T. ) ;
#2119 = EDGE_LOOP ( 'NONE', ( #5406, #333, #1859, #7797 ) ) ;
#2120 = LINE ( 'NONE', #932, #12211 ) ;
#2121 = VERTEX_POINT ( 'NONE', #6281 ) ;
#2122 = EDGE_CURVE ( 'NONE', #13543, #2746, #10722, .T. ) ;
#2123 = CARTESIAN_POINT ( 'NONE',  ( 0.3074992278157512304, 2.196686566159293807, -2.407412430484044816E-32 ) ) ;
#2124 = DIRECTION ( 'NONE',  ( 0.000000000000000000, 0.000000000000000000, -1.000000000000000000 ) ) ;
#2125 = CIRCLE ( 'NONE', #3735, 2.649999999999985700 ) ;
#2126 = B_SPLINE_CURVE_WITH_KNOTS ( 'NONE', 3,
 ( #8464, #10582, #12826, #10510, #3980, #9571, #13979, #4051 ),
 .UNSPECIFIED., .F., .F.,
 ( 4, 2, 2, 4 ),
 ( 0.000000000000000000, 0.002450665683189818828, 0.003675998524784728459, 0.004901331366379638524 ),
 .UNSPECIFIED. ) ;
#2127 = LINE ( 'NONE', #5400, #1772 ) ;
#2128 = CARTESIAN_POINT ( 'NONE',  ( 134.9999999999999432, -36.99999999999997868, 10.00000000000000178 ) ) ;
#2129 = MECHANICAL_DESIGN_GEOMETRIC_PRESENTATION_REPRESENTATION (  '', ( #10937 ), #13699 ) ;
#2130 = DIRECTION ( 'NONE',  ( -0.000000000000000000, -1.000000000000000000, -0.000000000000000000 ) ) ;
#2131 = DIRECTION ( 'NONE',  ( 1.000000000000000000, 0.000000000000000000, 0.000000000000000000 ) ) ;
#2132 = ORIENTED_EDGE ( 'NONE', *, *, #371, .T. ) ;
#2133 = ORIENTED_EDGE ( 'NONE', *, *, #10960, .F. ) ;
#2134 = AXIS2_PLACEMENT_3D ( 'NONE', #4026, #2935, #1689 ) ;
#2135 = PLANE ( 'NONE',  #31 ) ;
#2136 = AXIS2_PLACEMENT_3D ( 'NONE', #1777, #12880, #7511 ) ;
#2137 = ORIENTED_EDGE ( 'NONE', *, *, #7283, .T. ) ;
#2138 = LINE ( 'NONE', #952, #9182 ) ;
#2139 = VECTOR ( 'NONE', #1826, 1000.000000000000000 ) ;
#2140 = EDGE_CURVE ( 'NONE', #1008, #8392, #4629, .T. ) ;
#2141 = CARTESIAN_POINT ( 'NONE',  ( 5.000000000000000888, 0.000000000000000000, 0.000000000000000000 ) ) ;
#2142 = PRODUCT_DEFINITION ( 'UNKNOWN', '', #4249, #14046 ) ;
#2143 = DIRECTION ( 'NONE',  ( 1.000000000000000000, 0.000000000000000000, 0.000000000000000000 ) ) ;
#2144 = EDGE_LOOP ( 'NONE', ( #11697, #1713, #2037, #6971 ) ) ;
#2145 = AXIS2_PLACEMENT_3D ( 'NONE', #591, #5989, #12873 ) ;
#2146 = LINE ( 'NONE', #8746, #11857 ) ;
#2147 = DIRECTION ( 'NONE',  ( -0.000000000000000000, -0.000000000000000000, 1.000000000000000000 ) ) ;
#2148 = LINE ( 'NONE', #2289, #6717 ) ;
#2149 = DIRECTION ( 'NONE',  ( -1.000000000000000000, -0.000000000000000000, -0.000000000000000000 ) ) ;
#2150 = EDGE_CURVE ( 'NONE', #4208, #13509, #3942, .T. ) ;
#2151 = EDGE_CURVE ( 'NONE', #4585, #8933, #7405, .T. ) ;
#2152 = EDGE_LOOP ( 'NONE', ( #4708, #4758, #4849, #9813, #5810 ) ) ;
#2153 = EDGE_CURVE ( 'NONE', #4789, #11219, #8093, .T. ) ;
#2154 = DIRECTION ( 'NONE',  ( 0.000000000000000000, 0.4999999999999993339, -0.8660254037844390407 ) ) ;
#2155 = AXIS2_PLACEMENT_3D ( 'NONE', #8596, #14171, #9980 ) ;
#2156 = CARTESIAN_POINT ( 'NONE',  ( 2.500000000000000000, -2.357898499370432166, 3.035766082959412415E-15 ) ) ;
#2157 = DIRECTION ( 'NONE',  ( 1.000000000000000000, 0.000000000000000000, 0.000000000000000000 ) ) ;
#2158 = EDGE_LOOP ( 'NONE', ( #8217, #6367, #13265, #7040 ) ) ;
#2159 = LINE ( 'NONE', #4968, #8486 ) ;
#2160 = DIRECTION ( 'NONE',  ( 2.312964634635743450E-16, 1.000000000000000000, 0.000000000000000000 ) ) ;
#2161 = DIRECTION ( 'NONE',  ( -1.000000000000000000, 0.000000000000000000, -0.000000000000000000 ) ) ;
#2162 = DIRECTION ( 'NONE',  ( 1.000000000000000000, 6.123233995736766036E-17, -6.123233995736764803E-17 ) ) ;
#2163 = EDGE_CURVE ( 'NONE', #10673, #5456, #2738, .T. ) ;
#2164 = ADVANCED_FACE ( 'NONE', ( #11580 ), #12881, .T. ) ;
#2165 = VERTEX_POINT ( 'NONE', #8309 ) ;
#2166 = CARTESIAN_POINT ( 'NONE',  ( 228.6602540378443393, -80.00000000000007105, 50.00000000000001421 ) ) ;
#2167 = PRODUCT_DEFINITION_SHAPE ( 'NONE', 'NONE',  #5165 ) ;
#2168 = EDGE_LOOP ( 'NONE', ( #5649, #1457, #10994 ) ) ;
#2169 = DIRECTION ( 'NONE',  ( 0.000000000000000000, 0.000000000000000000, -1.000000000000000000 ) ) ;
#2170 = CARTESIAN_POINT ( 'NONE',  ( 470.0000000000000000, -20.00000000000000000, 250.0000000000000000 ) ) ;
#2171 = ADVANCED_FACE ( 'NONE', ( #9405 ), #8384, .F. ) ;
#2172 = ORIENTED_EDGE ( 'NONE', *, *, #10401, .F. ) ;
#2173 = EDGE_LOOP ( 'NONE', ( #1242, #179 ) ) ;
#2174 = DIRECTION ( 'NONE',  ( -1.000000000000000000, 0.000000000000000000, 0.000000000000000000 ) ) ;
#2175 = UNCERTAINTY_MEASURE_WITH_UNIT (LENGTH_MEASURE( 1.000000000000000082E-05 ), #11453, 'distance_accuracy_value', 'NONE');
#2176 = PLANE ( 'NONE',  #1754 ) ;
#2177 = FACE_OUTER_BOUND ( 'NONE', #9843, .T. ) ;
#2178 = DIRECTION ( 'NONE',  ( 1.000000000000000000, 0.000000000000000000, 0.000000000000000000 ) ) ;
#2179 = DIRECTION ( 'NONE',  ( 1.000000000000000000, 0.000000000000000000, 0.000000000000000000 ) ) ;
#2180 = FACE_OUTER_BOUND ( 'NONE', #10622, .T. ) ;
#2181 = DIRECTION ( 'NONE',  ( -0.000000000000000000, -1.000000000000000000, -0.000000000000000000 ) ) ;
#2182 = ITEM_DEFINED_TRANSFORMATION ( 'NONE', 'NONE', #5620,  #14039 ) ;
#2183 = LINE ( 'NONE', #856, #3860 ) ;
#2184 = EDGE_LOOP ( 'NONE', ( #7998, #13015, #10265, #7876 ) ) ;
#2185 = ORIENTED_EDGE ( 'NONE', *, *, #8419, .F. ) ;
#2186 = DIRECTION ( 'NONE',  ( -1.000000000000000000, -1.460819769243627131E-16, 0.000000000000000000 ) ) ;
#2187 = ORIENTED_EDGE ( 'NONE', *, *, #13580, .F. ) ;
#2188 = DIRECTION ( 'NONE',  ( 0.000000000000000000, -0.000000000000000000, 1.000000000000000000 ) ) ;
#2189 = ORIENTED_EDGE ( 'NONE', *, *, #13813, .F. ) ;
#2190 = ORIENTED_EDGE ( 'NONE', *, *, #13328, .T. ) ;
#2191 = CARTESIAN_POINT ( 'NONE',  ( 302.5000000000000000, -36.99999999999997868, -169.9999999999999716 ) ) ;
#2192 = ORIENTED_EDGE ( 'NONE', *, *, #5442, .F. ) ;
#2193 = FACE_OUTER_BOUND ( 'NONE', #10787, .T. ) ;
#2194 = CARTESIAN_POINT ( 'NONE',  ( 0.2500000000000002220, 4.898587196589412829E-16, -4.000000000000000000 ) ) ;
#2195 = DIRECTION ( 'NONE',  ( -0.000000000000000000, -0.000000000000000000, 1.000000000000000000 ) ) ;
#2196 = EDGE_CURVE ( 'NONE', #8622, #10379, #9772, .T. ) ;
#2197 = DIRECTION ( 'NONE',  ( 0.000000000000000000, -0.5000000000000011102, -0.8660254037844379305 ) ) ;
#2198 = DIRECTION ( 'NONE',  ( 0.000000000000000000, 1.000000000000000000, 0.000000000000000000 ) ) ;
#2199 = FACE_BOUND ( 'NONE', #9232, .T. ) ;
#2200 = CLOSED_SHELL ( 'NONE', ( #3269, #5695, #3723, #9080, #6131, #163, #11343, #8907, #4814, #1334, #2313, #976, #394, #799, #3827, #1130, #3012, #3741, #6245, #11618, #8182, #11286, #11248, #13792 ) ) ;
#2201 = ORIENTED_EDGE ( 'NONE', *, *, #5037, .T. ) ;
#2202 = ORIENTED_EDGE ( 'NONE', *, *, #8150, .T. ) ;
#2203 = DIRECTION ( 'NONE',  ( 0.000000000000000000, 0.000000000000000000, -1.000000000000000000 ) ) ;
#2204 = ORIENTED_EDGE ( 'NONE', *, *, #13849, .F. ) ;
#2205 = CARTESIAN_POINT ( 'NONE',  ( 145.5000000000000284, -95.00000000000008527, -190.0000000000000000 ) ) ;
#2206 = FACE_BOUND ( 'NONE', #10374, .T. ) ;
#2207 = LINE ( 'NONE', #3316, #9921 ) ;
#2208 = VERTEX_POINT ( 'NONE', #14179 ) ;
#2209 = CARTESIAN_POINT ( 'NONE',  ( 2.740000000000000213, 0.000000000000000000, 0.000000000000000000 ) ) ;
#2210 = AXIS2_PLACEMENT_3D ( 'NONE', #5378, #9807, #6534 ) ;
#2211 = DIRECTION ( 'NONE',  ( -1.000000000000000000, 0.000000000000000000, 0.000000000000000000 ) ) ;
#2212 = DIRECTION ( 'NONE',  ( -0.000000000000000000, -0.000000000000000000, 1.000000000000000000 ) ) ;
#2213 = DIRECTION ( 'NONE',  ( 1.000000000000000000, 0.000000000000000000, 0.000000000000000000 ) ) ;
#2214 = ADVANCED_FACE ( 'NONE', ( #7586 ), #2290, .F. ) ;
#2215 = VERTEX_POINT ( 'NONE', #4326 ) ;
#2216 = VECTOR ( 'NONE', #10603, 1000.000000000000000 ) ;
#2217 = ADVANCED_FACE ( 'NONE', ( #13247, #6644 ), #8752, .T. ) ;
#2218 = CONICAL_SURFACE ( 'NONE', #6152, 2.055000000000000160, 0.7853981633974639331 ) ;
#2219 = DIRECTION ( 'NONE',  ( 1.000000000000000000, 0.000000000000000000, 0.000000000000000000 ) ) ;
#2220 = CARTESIAN_POINT ( 'NONE',  ( 228.6602540378443393, -80.00000000000007105, 55.00000000000002132 ) ) ;
#2221 = FACE_BOUND ( 'NONE', #2786, .T. ) ;
#2222 = EDGE_LOOP ( 'NONE', ( #209, #9361, #13489, #1858 ) ) ;
#2223 = LINE ( 'NONE', #3397, #5479 ) ;
#2224 = EDGE_CURVE ( 'NONE', #12771, #8099, #3109, .T. ) ;
#2225 = VECTOR ( 'NONE', #13991, 1000.000000000000000 ) ;
#2226 = CYLINDRICAL_SURFACE ( 'NONE', #1529, 2.500000000000000888 ) ;
#2227 = DIRECTION ( 'NONE',  ( 1.000000000000000000, 0.000000000000000000, 0.000000000000000000 ) ) ;
#2228 = DIRECTION ( 'NONE',  ( -1.000000000000000000, 0.000000000000000000, 0.000000000000000000 ) ) ;
#2229 = EDGE_CURVE ( 'NONE', #2405, #6772, #8897, .T. ) ;
#2230 = EDGE_CURVE ( 'NONE', #5572, #10689, #13888, .T. ) ;
#2231 = ORIENTED_EDGE ( 'NONE', *, *, #7973, .T. ) ;
#2232=STYLED_ITEM('',(#14417),#8769);
#2233 = CARTESIAN_POINT ( 'NONE',  ( 197.5000000000000000, -90.00000000000007105, 55.00000000000001421 ) ) ;
#2234 = AXIS2_PLACEMENT_3D ( 'NONE', #1608, #12858, #732 ) ;
#2235 = EDGE_LOOP ( 'NONE', ( #7959, #3337, #5658, #10144, #1419 ) ) ;
#2236 = CARTESIAN_POINT ( 'NONE',  ( 219.9999999999999147, -85.00000000000009948, 0.000000000000000000 ) ) ;
#2237 = CIRCLE ( 'NONE', #1762, 9.999999999999980460 ) ;
#2238 = ORIENTED_EDGE ( 'NONE', *, *, #13328, .F. ) ;
#2239 = VERTEX_POINT ( 'NONE', #7655 ) ;
#2240 = FACE_OUTER_BOUND ( 'NONE', #13467, .T. ) ;
#2241 = EDGE_CURVE ( 'NONE', #3696, #7324, #4169, .T. ) ;
#2242 = EDGE_CURVE ( 'NONE', #161, #6979, #13421, .T. ) ;
#2243 = DIRECTION ( 'NONE',  ( -1.000000000000000000, 0.000000000000000000, -0.000000000000000000 ) ) ;
#2244 = VECTOR ( 'NONE', #1390, 1000.000000000000000 ) ;
#2245 = DIRECTION ( 'NONE',  ( 0.000000000000000000, -1.000000000000000000, 1.287488025362403787E-15 ) ) ;
#2246 = EDGE_CURVE ( 'NONE', #5301, #2366, #5556, .T. ) ;
#2247 = LINE ( 'NONE', #3420, #3118 ) ;
#2248 = AXIS2_PLACEMENT_3D ( 'NONE', #13499, #6762, #4521 ) ;
#2249 = DIRECTION ( 'NONE',  ( -0.000000000000000000, 1.000000000000000000, -0.000000000000000000 ) ) ;
#2250 = DIRECTION ( 'NONE',  ( -1.000000000000000000, 0.000000000000000000, 0.000000000000000000 ) ) ;
#2251 = SURFACE_SIDE_STYLE ('',( #1142 ) ) ;
#2252 = CARTESIAN_POINT ( 'NONE',  ( 303.3333333333333144, -15.00000000000000000, 222.5000000000000853 ) ) ;
#2253 = EDGE_CURVE ( 'NONE', #11549, #770, #1372, .T. ) ;
#2254 = VECTOR ( 'NONE', #9603, 1000.000000000000000 ) ;
#2255 = PLANE ( 'NONE',  #120 ) ;
#2256 = AXIS2_PLACEMENT_3D ( 'NONE', #11705, #8430, #7495 ) ;
#2257 = EDGE_LOOP ( 'NONE', ( #7508, #5212, #2594, #9324 ) ) ;
#2258 = ORIENTED_EDGE ( 'NONE', *, *, #2140, .F. ) ;
#2259 = PLANE ( 'NONE',  #4981 ) ;
#2260 = EDGE_LOOP ( 'NONE', ( #10953, #2981, #1033, #4159 ) ) ;
#2261 = CYLINDRICAL_SURFACE ( 'NONE', #3990, 2.649999999999985700 ) ;
#2262 = CIRCLE ( 'NONE', #7126, 2.649999999999985700 ) ;
#2263 = EDGE_LOOP ( 'NONE', ( #310, #8285, #6161, #4078 ) ) ;
#2264 = LINE ( 'NONE', #7836, #8506 ) ;
#2265 = ORIENTED_EDGE ( 'NONE', *, *, #5401, .F. ) ;
#2266 = CARTESIAN_POINT ( 'NONE',  ( 319.9999999999999432, -225.0010000000000048, -19.99999999999998934 ) ) ;
#2267 = AXIS2_PLACEMENT_3D ( 'NONE', #9991, #1263, #4486 ) ;
#2268 = CIRCLE ( 'NONE', #6202, 2.649999999999985700 ) ;
#2269 = DIRECTION ( 'NONE',  ( 0.000000000000000000, 0.000000000000000000, 1.000000000000000000 ) ) ;
#2270 = DIRECTION ( 'NONE',  ( 0.000000000000000000, 0.000000000000000000, -1.000000000000000000 ) ) ;
#2271 = DIRECTION ( 'NONE',  ( -0.000000000000000000, 0.000000000000000000, -1.000000000000000000 ) ) ;
#2272 = CARTESIAN_POINT ( 'NONE',  ( 0.000000000000000000, 2.357898499370431722, -2.818925648462311528E-15 ) ) ;
#2273 = MECHANICAL_DESIGN_GEOMETRIC_PRESENTATION_REPRESENTATION (  '', ( #5478 ), #12889 ) ;
#2274 = LINE ( 'NONE', #8661, #6193 ) ;
#2275 = SHAPE_REPRESENTATION ( 'pan head cross recess screw_iso_ISO 7045 - M5 x 25 - Z - 25N', ( #14039 ), #4225 ) ;
#2276 = VERTEX_POINT ( 'NONE', #5632 ) ;
#2277 = AXIS2_PLACEMENT_3D ( 'NONE', #7218, #5990, #9334 ) ;
#2278 = ORIENTED_EDGE ( 'NONE', *, *, #10271, .T. ) ;
#2279 = EDGE_CURVE ( 'NONE', #8841, #9866, #1840, .T. ) ;
#2280 = LINE ( 'NONE', #5410, #7244 ) ;
#2281 = VERTEX_POINT ( 'NONE', #10865 ) ;
#2282 = DIRECTION ( 'NONE',  ( 0.000000000000000000, 0.000000000000000000, 1.000000000000000000 ) ) ;
#2283 = FACE_OUTER_BOUND ( 'NONE', #2836, .T. ) ;
#2284 =( NAMED_UNIT ( * ) PLANE_ANGLE_UNIT ( ) SI_UNIT ( $, .RADIAN. ) );
#2285 = ORIENTED_EDGE ( 'NONE', *, *, #4791, .F. ) ;
#2286 = DIRECTION ( 'NONE',  ( -0.000000000000000000, -0.000000000000000000, 1.000000000000000000 ) ) ;
#2287 = AXIS2_PLACEMENT_3D ( 'NONE', #1914, #7279, #8436 ) ;
#2288 = CARTESIAN_POINT ( 'NONE',  ( 2.500000000000000000, 2.357898499370433054, -1.951563910473907981E-15 ) ) ;
#2289 = CARTESIAN_POINT ( 'NONE',  ( -132.3499999999999943, 45.00000000000001421, 30.00000000000000000 ) ) ;
#2290 = PLANE ( 'NONE',  #2305 ) ;
#2291 = ORIENTED_EDGE ( 'NONE', *, *, #13026, .F. ) ;
#2292 = EDGE_CURVE ( 'NONE', #1971, #4138, #8213, .T. ) ;
#2293 = VECTOR ( 'NONE', #10382, 1000.000000000000000 ) ;
#2294 = CARTESIAN_POINT ( 'NONE',  ( 5.200000000000002842, 0.000000000000000000, 0.000000000000000000 ) ) ;
#2295 = VECTOR ( 'NONE', #4438, 999.9999999999998863 ) ;
#2296 = CARTESIAN_POINT ( 'NONE',  ( -297.4999999999999432, -75.00000000000008527, 329.9999999999999432 ) ) ;
#2297 = DIRECTION ( 'NONE',  ( 0.000000000000000000, -0.000000000000000000, 1.000000000000000000 ) ) ;
#2298 = VERTEX_POINT ( 'NONE', #12150 ) ;
#2300 = EDGE_CURVE ( 'NONE', #14086, #931, #8673, .T. ) ;
#2299 = CARTESIAN_POINT ( 'NONE',  ( 4.000000000000000000, -1.942223658245635809, -0.3516579909967643691 ) ) ;
#2301 = CARTESIAN_POINT ( 'NONE',  ( -31.74999999999995737, 0.000000000000000000, 0.000000000000000000 ) ) ;
#2302 = DIRECTION ( 'NONE',  ( 0.000000000000000000, 0.000000000000000000, -1.000000000000000000 ) ) ;
#2303 = DIRECTION ( 'NONE',  ( 6.123233995736766036E-17, -1.000000000000000000, 0.000000000000000000 ) ) ;
#2304 = AXIS2_PLACEMENT_3D ( 'NONE', #2955, #6136, #748 ) ;
#2305 = AXIS2_PLACEMENT_3D ( 'NONE', #7725, #2213, #12228 ) ;
#2306 = ORIENTED_EDGE ( 'NONE', *, *, #11640, .T. ) ;
#2307 = CARTESIAN_POINT ( 'NONE',  ( 4.000000000000000000, 2.309401076758497151, -3.433295621305379353 ) ) ;
#2308 = ORIENTED_EDGE ( 'NONE', *, *, #13568, .T. ) ;
#2309 = DIRECTION ( 'NONE',  ( -0.000000000000000000, -0.000000000000000000, 1.000000000000000000 ) ) ;
#2310 = EDGE_LOOP ( 'NONE', ( #10390, #4973 ) ) ;
#2311 = ORIENTED_EDGE ( 'NONE', *, *, #8590, .F. ) ;
#2313 = ADVANCED_FACE ( 'NONE', ( #8604 ), #5418, .T. ) ;
#2312 = DIRECTION ( 'NONE',  ( -0.000000000000000000, -0.000000000000000000, 1.000000000000000000 ) ) ;
#2314 = PRODUCT_RELATED_PRODUCT_CATEGORY ( 'part', '', ( #11441 ) ) ;
#2315 = CARTESIAN_POINT ( 'NONE',  ( 2.500000000000000000, -1.178949249685213863, 2.042000000000002924 ) ) ;
#2316 = AXIS2_PLACEMENT_3D ( 'NONE', #9483, #381, #12666 ) ;
#2317 = DIRECTION ( 'NONE',  ( 0.000000000000000000, 0.000000000000000000, -1.000000000000000000 ) ) ;
#2318 = AXIS2_PLACEMENT_3D ( 'NONE', #3055, #7467, #14038 ) ;
#2319 = DIRECTION ( 'NONE',  ( 1.000000000000000000, 0.000000000000000000, 0.000000000000000000 ) ) ;
#2320 = LINE ( 'NONE', #12259, #3984 ) ;
#2321 = DIRECTION ( 'NONE',  ( -0.000000000000000000, -0.000000000000000000, -1.000000000000000000 ) ) ;
#2322 = FILL_AREA_STYLE_COLOUR ( '', #10495 ) ;
#2323 = COLOUR_RGB ( '',0.8941176470588234615, 0.8941176470588234615, 0.8941176470588234615 ) ;
#2324 = CARTESIAN_POINT ( 'NONE',  ( 5.000000000000002665, 3.306546357697854226E-16, 2.700000000000000622 ) ) ;
#2325 = CARTESIAN_POINT ( 'NONE',  ( 8.000000000000000000, 0.5150000000000000133, 1.798112889504231112E-15 ) ) ;
#2326 = EDGE_LOOP ( 'NONE', ( #10559, #6317, #1076, #2403 ) ) ;
#2327 = VERTEX_POINT ( 'NONE', #962 ) ;
#2328 = ADVANCED_FACE ( 'NONE', ( #9841 ), #14248, .F. ) ;
#2329 = EDGE_CURVE ( 'NONE', #3772, #12248, #11464, .T. ) ;
#2330 = DIRECTION ( 'NONE',  ( -0.000000000000000000, -0.000000000000000000, -1.000000000000000000 ) ) ;
#2331 = VECTOR ( 'NONE', #3546, 1000.000000000000000 ) ;
#2332 =( REPRESENTATION_RELATIONSHIP ('NONE','NONE', #11251, #13104 ) REPRESENTATION_RELATIONSHIP_WITH_TRANSFORMATION ( #5940 )SHAPE_REPRESENTATION_RELATIONSHIP( ) );
#2333 = ORIENTED_EDGE ( 'NONE', *, *, #4805, .T. ) ;
#2334 = EDGE_CURVE ( 'NONE', #2529, #12855, #12370, .T. ) ;
#2335 = DIRECTION ( 'NONE',  ( -0.000000000000000000, -0.000000000000000000, 1.000000000000000000 ) ) ;
#2336 = VERTEX_POINT ( 'NONE', #4687 ) ;
#2337 = CARTESIAN_POINT ( 'NONE',  ( 0.06760930072668812352, 0.5150000000000032330, -0.9010842325122888630 ) ) ;
#2338 = VERTEX_POINT ( 'NONE', #4611 ) ;
#2339 = AXIS2_PLACEMENT_3D ( 'NONE', #541, #6227, #9420 ) ;
#2340 = CARTESIAN_POINT ( 'NONE',  ( 470.0000000000000000, 0.000000000000000000, 205.0000000000000284 ) ) ;
#2341 = CARTESIAN_POINT ( 'NONE',  ( 134.9999999999999432, -56.99999999999997158, 10.00000000000000000 ) ) ;
#2342 = DIRECTION ( 'NONE',  ( -0.000000000000000000, -1.000000000000000000, -0.000000000000000000 ) ) ;
#2343 = CARTESIAN_POINT ( 'NONE',  ( 242.5000000000000000, -90.00000000000007105, 55.00000000000001421 ) ) ;
#2344 = AXIS2_PLACEMENT_3D ( 'NONE', #13518, #3808, #3597 ) ;
#2345 = CARTESIAN_POINT ( 'NONE',  ( 303.3333333333333144, -20.00000000000000000, 225.1500000000000625 ) ) ;
#2346 = DIRECTION ( 'NONE',  ( 1.000000000000000000, 0.000000000000000000, 6.123233995736766036E-17 ) ) ;
#2347 = DIRECTION ( 'NONE',  ( 1.000000000000000000, 0.000000000000000000, 0.000000000000000000 ) ) ;
#2348 = ORIENTED_EDGE ( 'NONE', *, *, #1480, .F. ) ;
#2349 = AXIS2_PLACEMENT_3D ( 'NONE', #4901, #7139, #10404 ) ;
#2350 = ORIENTED_EDGE ( 'NONE', *, *, #13834, .F. ) ;
#2351 = VERTEX_POINT ( 'NONE', #11355 ) ;
#2352 = DIRECTION ( 'NONE',  ( 0.000000000000000000, 1.000000000000000000, 0.000000000000000000 ) ) ;
#2353 = AXIS2_PLACEMENT_3D ( 'NONE', #8008, #11506, #5993 ) ;
#2354 = ORIENTED_EDGE ( 'NONE', *, *, #6579, .T. ) ;
#2355 = DIRECTION ( 'NONE',  ( 1.000000000000000000, 0.000000000000000000, 0.000000000000000000 ) ) ;
#2356 = DIRECTION ( 'NONE',  ( 0.000000000000000000, -0.000000000000000000, -1.000000000000000000 ) ) ;
#2357 = CARTESIAN_POINT ( 'NONE',  ( 140.0000000000000000, -75.00000000000008527, 169.9999999999999716 ) ) ;
#2358 =( BOUNDED_SURFACE ( )  B_SPLINE_SURFACE ( 3, 2, ( 
 ( #5514, #9869, #4431 ),
 ( #14277, #6741, #13121 ),
 ( #5716, #12466, #4717 ),
 ( #12539, #1564, #9127 ),
 ( #1491, #9352, #2531 ),
 ( #6810, #8101, #11520 ) ),
 .UNSPECIFIED., .F., .F., .T. ) 
 B_SPLINE_SURFACE_WITH_KNOTS ( ( 4, 2, 4 ),
 ( 3, 3 ),
 ( 0.02032853247518126918, 0.02278863295364821906, 0.02524873343211516893 ),
 ( 0.000000000000000000, 1.000000000000000000 ),
 .UNSPECIFIED. ) 
 GEOMETRIC_REPRESENTATION_ITEM ( )  RATIONAL_B_SPLINE_SURFACE ( (
 ( 1.000000000000000000, 0.8047781615896838492, 1.000000000000000000),
 ( 1.000000000000000000, 0.8123767586288186404, 1.000000000000000000),
 ( 1.000000000000000000, 0.8190662415565814758, 1.000000000000000000),
 ( 1.000000000000000000, 0.8192361015667604107, 1.000000000000000000),
 ( 1.000000000000000000, 0.8126135807104967190, 1.000000000000000000),
 ( 1.000000000000000000, 0.8047712338318580017, 1.000000000000000000) ) ) 
 REPRESENTATION_ITEM ( '' )  SURFACE ( )  );
#2359 = DIRECTION ( 'NONE',  ( -1.000000000000000000, 0.000000000000000000, -0.000000000000000000 ) ) ;
#2360 = EDGE_CURVE ( 'NONE', #3993, #5384, #5763, .T. ) ;
#2361 = LINE ( 'NONE', #11077, #11596 ) ;
#2362 = DIRECTION ( 'NONE',  ( 1.000000000000000000, 0.000000000000000000, 0.000000000000000000 ) ) ;
#2363 = AXIS2_PLACEMENT_3D ( 'NONE', #9130, #4720, #4646 ) ;
#2364 = DIRECTION ( 'NONE',  ( 0.000000000000000000, 0.000000000000000000, -1.000000000000000000 ) ) ;
#2365 = VECTOR ( 'NONE', #2020, 1000.000000000000000 ) ;
#2366 = VERTEX_POINT ( 'NONE', #1398 ) ;
#2367 = AXIS2_PLACEMENT_3D ( 'NONE', #12240, #4419, #13321 ) ;
#2368 = CARTESIAN_POINT ( 'NONE',  ( 303.3333333333333144, -20.00000000000000000, 225.1500000000000625 ) ) ;
#2369 = DIRECTION ( 'NONE',  ( 0.000000000000000000, 0.000000000000000000, 1.000000000000000000 ) ) ;
#2370 = VECTOR ( 'NONE', #12374, 1000.000000000000000 ) ;
#2371 = DIRECTION ( 'NONE',  ( -1.000000000000000000, 0.000000000000000000, 0.000000000000000000 ) ) ;
#2372 = VERTEX_POINT ( 'NONE', #10329 ) ;
#2373 = AXIS2_PLACEMENT_3D ( 'NONE', #1628, #377, #10421 ) ;
#2374 = DIRECTION ( 'NONE',  ( 1.000000000000000000, 0.000000000000000000, 0.000000000000000000 ) ) ;
#2375 = EDGE_CURVE ( 'NONE', #9732, #1808, #1728, .T. ) ;
#2376 = AXIS2_PLACEMENT_3D ( 'NONE', #4730, #2543, #262 ) ;
#2377 = DIRECTION ( 'NONE',  ( 1.000000000000000000, 0.000000000000000000, 0.000000000000000000 ) ) ;
#2378 = DIRECTION ( 'NONE',  ( 1.000000000000000000, 0.000000000000000000, 0.000000000000000000 ) ) ;
#2379 = ORIENTED_EDGE ( 'NONE', *, *, #5447, .F. ) ;
#2380 = EDGE_CURVE ( 'NONE', #9549, #4302, #12862, .T. ) ;
#2381 = LINE ( 'NONE', #12383, #7990 ) ;
#2382 = PRODUCT_DEFINITION_FORMATION_WITH_SPECIFIED_SOURCE ( 'ANY', '', #1347, .NOT_KNOWN. ) ;
#2383 = ORIENTED_EDGE ( 'NONE', *, *, #12018, .T. ) ;
#2384 = CARTESIAN_POINT ( 'NONE',  ( 1.999999999999998668, 1.249139735130300365E-15, 10.20000000000000107 ) ) ;
#2385 = ORIENTED_EDGE ( 'NONE', *, *, #14034, .F. ) ;
#2386 = EDGE_LOOP ( 'NONE', ( #13176, #9459 ) ) ;
#2387 = CYLINDRICAL_SURFACE ( 'NONE', #13806, 2.500000000000002220 ) ;
#2388 = CARTESIAN_POINT ( 'NONE',  ( 203.5000000000000000, -85.00000000000007105, 50.00000000000001421 ) ) ;
#2389 = VECTOR ( 'NONE', #11604, 1000.000000000000000 ) ;
#2390 = CARTESIAN_POINT ( 'NONE',  ( 1.799999999999996048, 0.000000000000000000, 0.000000000000000000 ) ) ;
#2391 = LINE ( 'NONE', #12469, #1159 ) ;
#2392 = DIRECTION ( 'NONE',  ( 0.000000000000000000, 0.000000000000000000, 1.000000000000000000 ) ) ;
#2393 = CARTESIAN_POINT ( 'NONE',  ( 0.000000000000000000, -1.178949249685213863, 2.042000000000002924 ) ) ;
#2394 = FILL_AREA_STYLE ('',( #997 ) ) ;
#2395 = DIRECTION ( 'NONE',  ( 0.000000000000000000, -1.000000000000000000, 0.000000000000000000 ) ) ;
#2396 = ORIENTED_EDGE ( 'NONE', *, *, #6668, .F. ) ;
#2397 = VERTEX_POINT ( 'NONE', #13376 ) ;
#2398 = ADVANCED_FACE ( 'NONE', ( #11282, #6923, #6996, #11429 ), #1471, .F. ) ;
#2399 = LINE ( 'NONE', #4512, #13534 ) ;
#2400 = ADVANCED_FACE ( 'NONE', ( #12300 ), #361, .F. ) ;
#2401 = ORIENTED_EDGE ( 'NONE', *, *, #6755, .F. ) ;
#2402 = LINE ( 'NONE', #9137, #4242 ) ;
#2403 = ORIENTED_EDGE ( 'NONE', *, *, #2229, .T. ) ;
#2404 = CARTESIAN_POINT ( 'NONE',  ( 134.9999999999999432, -56.99999999999997158, 0.000000000000000000 ) ) ;
#2405 = VERTEX_POINT ( 'NONE', #12584 ) ;
#2406 = DIRECTION ( 'NONE',  ( -0.000000000000000000, -0.000000000000000000, 1.000000000000000000 ) ) ;
#2407 = PRODUCT ( 'socket head cap screw_iso_ISO 4762 M5 x 12 - 12N', 'socket head cap screw_iso_ISO 4762 M5 x 12 - 12N', '', ( #3177 ) ) ;
#2408 = CARTESIAN_POINT ( 'NONE',  ( -144.9999999999999432, -105.0000000000000853, 30.00000000000000000 ) ) ;
#2409 = CARTESIAN_POINT ( 'NONE',  ( -20.63749999999999929, 1.224646799147352862E-15, 9.999999999999996447 ) ) ;
#2410 = EDGE_CURVE ( 'NONE', #3237, #12266, #1967, .T. ) ;
#2411 = DIRECTION ( 'NONE',  ( 0.000000000000000000, 0.000000000000000000, -1.000000000000000000 ) ) ;
#2412 = PRESENTATION_STYLE_ASSIGNMENT (( #10039 ) ) ;
#2413 = DIRECTION ( 'NONE',  ( 1.000000000000000000, 0.000000000000000000, 6.123233995736766036E-17 ) ) ;
#2414 = DIRECTION ( 'NONE',  ( 1.000000000000000000, 0.000000000000000000, 0.000000000000000000 ) ) ;
#2415 = ORIENTED_EDGE ( 'NONE', *, *, #10083, .F. ) ;
#2416 = ADVANCED_FACE ( 'NONE', ( #3526 ), #13664, .T. ) ;
#2417 = VERTEX_POINT ( 'NONE', #11493 ) ;
#2418 = VERTEX_POINT ( 'NONE', #4540 ) ;
#2419 = DIRECTION ( 'NONE',  ( -1.000000000000000000, 0.000000000000000000, -0.000000000000000000 ) ) ;
#2420 = ORIENTED_EDGE ( 'NONE', *, *, #8634, .T. ) ;
#2421 = CARTESIAN_POINT ( 'NONE',  ( 0.000000000000000000, 0.000000000000000000, 200.0000000000000000 ) ) ;
#2422 = CARTESIAN_POINT ( 'NONE',  ( -302.4999999999999432, -75.00000000000008527, 0.000000000000000000 ) ) ;
#2423 = CARTESIAN_POINT ( 'NONE',  ( 299.9999999999999432, -75.00000000000008527, -186.2999999999999829 ) ) ;
#2424 = EDGE_CURVE ( 'NONE', #8882, #10563, #11943, .T. ) ;
#2425 = CLOSED_SHELL ( 'NONE', ( #10182, #6516, #327, #4010, #2688, #6499, #8614, #3759, #10923, #6035, #2848, #7603, #6053, #7191, #13852, #1496, #1930, #11232, #426, #7203, #10827, #643, #7016, #8801, #4439, #81, #37, #8347, #12972, #3378, #9001, #2795, #9488, #5963, #13581, #560, #7381, #9658, #156, #7500, #3144, #4173 ) ) ;
#2426 = CARTESIAN_POINT ( 'NONE',  ( -20.63749999999999574, 0.000000000000000000, 0.000000000000000000 ) ) ;
#2427 = ADVANCED_FACE ( 'NONE', ( #10190 ), #2508, .F. ) ;
#2428 = CARTESIAN_POINT ( 'NONE',  ( 2.500000000000000000, 0.000000000000000000, 0.000000000000000000 ) ) ;
#2429 = CARTESIAN_POINT ( 'NONE',  ( 20.55500000000001748, 0.000000000000000000, 0.000000000000000000 ) ) ;
#2430 = DIRECTION ( 'NONE',  ( -1.000000000000000000, 0.000000000000000000, 0.000000000000000000 ) ) ;
#2431 = EDGE_CURVE ( 'NONE', #770, #11549, #14243, .T. ) ;
#2432 = ORIENTED_EDGE ( 'NONE', *, *, #878, .T. ) ;
#2433 = AXIS2_PLACEMENT_3D ( 'NONE', #9250, #3732, #10118 ) ;
#2434 = DIRECTION ( 'NONE',  ( 1.000000000000000000, 0.000000000000000000, 0.000000000000000000 ) ) ;
#2435 = CARTESIAN_POINT ( 'NONE',  ( 444.9999999999999432, 8.660254037844390851, 200.0000000000000000 ) ) ;
#2436 = CARTESIAN_POINT ( 'NONE',  ( 79.99999999999971578, 35.00000000000000000, 10.00000000000000000 ) ) ;
#2437 = VERTEX_POINT ( 'NONE', #8958 ) ;
#2438 = DIRECTION ( 'NONE',  ( -1.000000000000000000, 0.000000000000000000, 0.000000000000000000 ) ) ;
#2439 = VECTOR ( 'NONE', #5459, 1000.000000000000000 ) ;
#2440 = LINE ( 'NONE', #9038, #8558 ) ;
#2441 = DIRECTION ( 'NONE',  ( -1.000000000000000000, -6.123233995736766036E-17, -6.123233995736764803E-17 ) ) ;
#2442 = VECTOR ( 'NONE', #2980, 1000.000000000000000 ) ;
#2443 = EDGE_CURVE ( 'NONE', #12248, #3772, #2661, .T. ) ;
#2444 = ORIENTED_EDGE ( 'NONE', *, *, #2929, .T. ) ;
#2445 = DIRECTION ( 'NONE',  ( 1.000000000000000000, 0.000000000000000000, 0.000000000000000000 ) ) ;
#2446 = ORIENTED_EDGE ( 'NONE', *, *, #5628, .F. ) ;
#2447 = EDGE_CURVE ( 'NONE', #6099, #11786, #4990, .T. ) ;
#2448 = DIRECTION ( 'NONE',  ( -0.000000000000000000, -0.000000000000000000, 1.000000000000000000 ) ) ;
#2449 = AXIS2_PLACEMENT_3D ( 'NONE', #4141, #989, #12044 ) ;
#2450 = ORIENTED_EDGE ( 'NONE', *, *, #972, .T. ) ;
#2451 = ORIENTED_EDGE ( 'NONE', *, *, #1391, .F. ) ;
#2452 = LINE ( 'NONE', #12178, #4315 ) ;
#2453 = CARTESIAN_POINT ( 'NONE',  ( 4.140404888673277384, 2.228338276487440428, -3.686887068327033390 ) ) ;
#2454 = CARTESIAN_POINT ( 'NONE',  ( -5.000000000000000888, 8.660254037844390851, 210.0000000000000000 ) ) ;
#2455 = CARTESIAN_POINT ( 'NONE',  ( 136.6666666666666288, -20.00000000000000000, 219.8500000000001080 ) ) ;
#2456 = CARTESIAN_POINT ( 'NONE',  ( 2.500000000000000000, 1.178949249685212974, -2.042000000000001148 ) ) ;
#2457 = CARTESIAN_POINT ( 'NONE',  ( 134.9999999999999716, 45.00000000000001421, 0.000000000000000000 ) ) ;
#2458 = SHAPE_REPRESENTATION_RELATIONSHIP ( 'NONE' , 'NONE' ,  #2275, #6456 ) ;
#2459 = VECTOR ( 'NONE', #5445, 1000.000000000000114 ) ;
#2460 = DIRECTION ( 'NONE',  ( 0.000000000000000000, 0.000000000000000000, 1.000000000000000000 ) ) ;
#2461 = CONTEXT_DEPENDENT_SHAPE_REPRESENTATION ( #10488, #10889 ) ;
#2462 = AXIS2_PLACEMENT_3D ( 'NONE', #4826, #4337, #8760 ) ;
#2463 = ORIENTED_EDGE ( 'NONE', *, *, #11515, .T. ) ;
#2464 = VERTEX_POINT ( 'NONE', #4385 ) ;
#2465 = VECTOR ( 'NONE', #6841, 1000.000000000000000 ) ;
#2466 = LINE ( 'NONE', #1442, #1966 ) ;
#2467 = ADVANCED_FACE ( 'NONE', ( #6699 ), #1235, .F. ) ;
#2468 = ORIENTED_EDGE ( 'NONE', *, *, #13310, .F. ) ;
#2469 = DIRECTION ( 'NONE',  ( 0.000000000000000000, 1.000000000000000000, 0.000000000000000000 ) ) ;
#2470 = AXIS2_PLACEMENT_3D ( 'NONE', #11242, #1282, #9061 ) ;
#2471 = VERTEX_POINT ( 'NONE', #7770 ) ;
#2472 = DIRECTION ( 'NONE',  ( -1.000000000000000000, 0.000000000000000000, 0.000000000000000000 ) ) ;
#2473 = EDGE_LOOP ( 'NONE', ( #13133, #1209, #9047, #6416 ) ) ;
#2475 = DIRECTION ( 'NONE',  ( 1.000000000000000000, 2.478176394252579538E-17, 0.000000000000000000 ) ) ;
#2474 = CONICAL_SURFACE ( 'NONE', #13125, 2.500000000000002220, 1.029744260000002631 ) ;
#2476 = CIRCLE ( 'NONE', #12423, 2.649999999999985700 ) ;
#2477 = DIRECTION ( 'NONE',  ( -0.000000000000000000, -0.000000000000000000, -1.000000000000000000 ) ) ;
#2478 = CARTESIAN_POINT ( 'NONE',  ( 2.500000000000000000, 1.178949249685213863, -2.042000000000001148 ) ) ;
#2479 = EDGE_CURVE ( 'NONE', #5504, #1662, #3149, .T. ) ;
#2480 = CIRCLE ( 'NONE', #7799, 4.556291390728477886 ) ;
#2481 = FACE_OUTER_BOUND ( 'NONE', #7158, .T. ) ;
#2482 = CIRCLE ( 'NONE', #2726, 0.2500000000000002220 ) ;
#2483 = ADVANCED_FACE ( 'NONE', ( #10038 ), #9155, .T. ) ;
#2484 = FILL_AREA_STYLE_COLOUR ( '', #8 ) ;
#2485 = DIRECTION ( 'NONE',  ( 1.000000000000000000, 0.000000000000000000, 6.123233995736766036E-17 ) ) ;
#2486 = DIRECTION ( 'NONE',  ( 0.000000000000000000, 0.000000000000000000, 1.000000000000000000 ) ) ;
#2487 = VECTOR ( 'NONE', #12138, 1000.000000000000000 ) ;
#2488 = VERTEX_POINT ( 'NONE', #5671 ) ;
#2489 = ORIENTED_EDGE ( 'NONE', *, *, #4088, .F. ) ;
#2490 = COLOUR_RGB ( '',1.000000000000000000, 0.9490196078431372140, 0.9098039215686274384 ) ;
#2491 = ORIENTED_EDGE ( 'NONE', *, *, #9692, .F. ) ;
#2492 = CARTESIAN_POINT ( 'NONE',  ( 5.200000000000002842, 3.061616997868384127E-16, -2.500000000000000888 ) ) ;
#2493 = TOROIDAL_SURFACE ( 'NONE', #2267, 11.75000000000000000, 1.050000000000000266 ) ;
#2494 = AXIS2_PLACEMENT_3D ( 'NONE', #6531, #10073, #104 ) ;
#2495 = ORIENTED_EDGE ( 'NONE', *, *, #9341, .T. ) ;
#2496 = CARTESIAN_POINT ( 'NONE',  ( 0.000000000000000000, 0.000000000000000000, 0.000000000000000000 ) ) ;
#2497 = ORIENTED_EDGE ( 'NONE', *, *, #12527, .F. ) ;
#2498 = FACE_OUTER_BOUND ( 'NONE', #2653, .T. ) ;
#2499 = CARTESIAN_POINT ( 'NONE',  ( -30.00000000000002842, -225.0000000000000000, 169.9999999999999716 ) ) ;
#2500 = VECTOR ( 'NONE', #9950, 1000.000000000000000 ) ;
#2501 = B_SPLINE_CURVE_WITH_KNOTS ( 'NONE', 3,
 ( #11126, #1161, #5398, #14229, #8939, #10036 ),
 .UNSPECIFIED., .F., .F.,
 ( 4, 2, 4 ),
 ( 0.000000000000000000, 0.0002095117440864783663, 0.0004190234881729567326 ),
 .UNSPECIFIED. ) ;
#2502 = ADVANCED_FACE ( 'NONE', ( #1014 ), #3376, .F. ) ;
#2503 = EDGE_CURVE ( 'NONE', #3958, #258, #9010, .T. ) ;
#2504 = CIRCLE ( 'NONE', #10359, 7.864440107515430434 ) ;
#2505 = LINE ( 'NONE', #6918, #8854 ) ;
#2506 = LINE ( 'NONE', #11639, #8355 ) ;
#2507 = LINE ( 'NONE', #3524, #6486 ) ;
#2508 = CYLINDRICAL_SURFACE ( 'NONE', #7524, 2.649999999999985700 ) ;
#2509 = ORIENTED_EDGE ( 'NONE', *, *, #13670, .T. ) ;
#2510 = ADVANCED_FACE ( 'NONE', ( #3508 ), #4297, .T. ) ;
#2511 = EDGE_CURVE ( 'NONE', #6112, #8606, #7297, .T. ) ;
#2512 = FILL_AREA_STYLE ('',( #5766 ) ) ;
#2513 = EDGE_CURVE ( 'NONE', #13072, #981, #4528, .T. ) ;
#2514 = DIRECTION ( 'NONE',  ( 0.000000000000000000, -1.000000000000000000, -3.491481338843133355E-15 ) ) ;
#2515 = DIRECTION ( 'NONE',  ( 0.8949343913984706411, 1.557891129246106293E-15, -0.4461977533473793778 ) ) ;
#2516 = DIRECTION ( 'NONE',  ( -1.000000000000000000, 0.000000000000000000, 0.000000000000000000 ) ) ;
#2517 = VERTEX_POINT ( 'NONE', #4523 ) ;
#2518 = CARTESIAN_POINT ( 'NONE',  ( -10.00000000000000000, 0.000000000000000000, 200.0000000000000000 ) ) ;
#2519 = FACE_OUTER_BOUND ( 'NONE', #4094, .T. ) ;
#2520 = CARTESIAN_POINT ( 'NONE',  ( 88.00000000000000000, 0.000000000000000000, 0.000000000000000000 ) ) ;
#2521 =( REPRESENTATION_RELATIONSHIP ('NONE','NONE', #11251, #13104 ) REPRESENTATION_RELATIONSHIP_WITH_TRANSFORMATION ( #1498 )SHAPE_REPRESENTATION_RELATIONSHIP( ) );
#2522 = EDGE_LOOP ( 'NONE', ( #5728, #3688, #4350, #7774 ) ) ;
#2523 = CIRCLE ( 'NONE', #2058, 2.500000000000000000 ) ;
#2524 = CARTESIAN_POINT ( 'NONE',  ( 137.6499999999999773, 45.00000000000001421, 10.00000000000000000 ) ) ;
#2525 = PRODUCT_DEFINITION_SHAPE ( 'NONE', 'NONE',  #14307 ) ;
#2526 = ORIENTED_EDGE ( 'NONE', *, *, #10124, .T. ) ;
#2527 = PLANE ( 'NONE',  #10913 ) ;
#2528 = ORIENTED_EDGE ( 'NONE', *, *, #8434, .F. ) ;
#2529 = VERTEX_POINT ( 'NONE', #129 ) ;
#2530 = FACE_OUTER_BOUND ( 'NONE', #13466, .T. ) ;
#2531 = CARTESIAN_POINT ( 'NONE',  ( -0.6810597143197697489, -4.461075778259609770, -3.598441714920717516 ) ) ;
#2532 = CARTESIAN_POINT ( 'NONE',  ( 53.33333333333330017, -14.99999999999999822, 225.1500000000000625 ) ) ;
#2533 = VECTOR ( 'NONE', #11742, 1000.000000000000000 ) ;
#2534 = DIRECTION ( 'NONE',  ( -0.000000000000000000, -0.000000000000000000, 1.000000000000000000 ) ) ;
#2535 = LINE ( 'NONE', #5794, #9550 ) ;
#2536 = DIRECTION ( 'NONE',  ( -9.912705577010325549E-17, 1.000000000000000000, 0.000000000000000000 ) ) ;
#2537 = EDGE_CURVE ( 'NONE', #1111, #4205, #10637, .T. ) ;
#2538 = DIRECTION ( 'NONE',  ( -0.000000000000000000, 1.000000000000000000, -0.000000000000000000 ) ) ;
#2539 = ORIENTED_EDGE ( 'NONE', *, *, #10370, .F. ) ;
#2540 = VERTEX_POINT ( 'NONE', #12002 ) ;
#2541 = CARTESIAN_POINT ( 'NONE',  ( 0.2500000000000002220, 0.000000000000000000, 4.250000000000000000 ) ) ;
#2542 = VERTEX_POINT ( 'NONE', #939 ) ;
#2543 = DIRECTION ( 'NONE',  ( -0.000000000000000000, -0.000000000000000000, -1.000000000000000000 ) ) ;
#2544 = VECTOR ( 'NONE', #7995, 1000.000000000000000 ) ;
#2545 = AXIS2_PLACEMENT_3D ( 'NONE', #3756, #1709, #7299 ) ;
#2546 = EDGE_LOOP ( 'NONE', ( #3601, #2044, #10898, #13528 ) ) ;
#2547 = DIRECTION ( 'NONE',  ( -1.000000000000000000, 0.000000000000000000, 0.000000000000000000 ) ) ;
#2548 = ORIENTED_EDGE ( 'NONE', *, *, #8156, .F. ) ;
#2549 = AXIS2_PLACEMENT_3D ( 'NONE', #11659, #5286, #9704 ) ;
#2550 = CARTESIAN_POINT ( 'NONE',  ( 124.9999999999999858, 55.00000000000000711, 10.00000000000000000 ) ) ;
#2551 = FACE_OUTER_BOUND ( 'NONE', #6774, .T. ) ;
#2552 = EDGE_LOOP ( 'NONE', ( #4449, #1463, #8826, #1580 ) ) ;
#2553 = PRESENTATION_LAYER_ASSIGNMENT (  '', '', ( #10000 ) ) ;
#2554 = CARTESIAN_POINT ( 'NONE',  ( 5.200000000000002842, 0.000000000000000000, 2.500000000000000444 ) ) ;
#2555 = CARTESIAN_POINT ( 'NONE',  ( 2.740000000000000213, 0.000000000000000000, 0.000000000000000000 ) ) ;
#2556 = PRESENTATION_STYLE_ASSIGNMENT (( #490 ) ) ;
#2557 =( NAMED_UNIT ( * ) PLANE_ANGLE_UNIT ( ) SI_UNIT ( $, .RADIAN. ) );
#2558 = APPLICATION_PROTOCOL_DEFINITION ( 'draft international standard', 'automotive_design', 1998, #7296 ) ;
#2559 = CARTESIAN_POINT ( 'NONE',  ( 233.9999999999999432, -85.00000000000007105, 180.0000000000000000 ) ) ;
#2560 = ORIENTED_EDGE ( 'NONE', *, *, #3697, .T. ) ;
#2561 = AXIS2_PLACEMENT_3D ( 'NONE', #4890, #10391, #19 ) ;
#2562 = ORIENTED_EDGE ( 'NONE', *, *, #14102, .T. ) ;
#2563 = VERTEX_POINT ( 'NONE', #4593 ) ;
#2564 = CIRCLE ( 'NONE', #12753, 7.983406227920510467 ) ;
#2565 = DIRECTION ( 'NONE',  ( 1.000000000000000000, 0.000000000000000000, 0.000000000000000000 ) ) ;
#2566 = EDGE_CURVE ( 'NONE', #4150, #298, #9941, .T. ) ;
#2567 = ORIENTED_EDGE ( 'NONE', *, *, #5765, .F. ) ;
#2568 = LINE ( 'NONE', #9382, #5482 ) ;
#2569 = VERTEX_POINT ( 'NONE', #7842 ) ;
#2570 = DIRECTION ( 'NONE',  ( 0.000000000000000000, -1.000000000000000000, -1.652937667529658626E-16 ) ) ;
#2571 = LINE ( 'NONE', #11559, #11541 ) ;
#2572 = CIRCLE ( 'NONE', #10684, 2.500000000000002220 ) ;
#2573 = FACE_OUTER_BOUND ( 'NONE', #9828, .T. ) ;
#2574 = DIRECTION ( 'NONE',  ( 0.000000000000000000, -1.000000000000000000, 0.000000000000000000 ) ) ;
#2575 = CIRCLE ( 'NONE', #690, 2.500000000000002220 ) ;
#2576 = CARTESIAN_POINT ( 'NONE',  ( 305.0000000000000000, -56.99999999999997158, -169.9999999999999716 ) ) ;
#2577 = DIRECTION ( 'NONE',  ( -0.000000000000000000, -0.000000000000000000, -1.000000000000000000 ) ) ;
#2578 = DIRECTION ( 'NONE',  ( -1.000000000000000000, 0.000000000000000000, 0.000000000000000000 ) ) ;
#2579 = ORIENTED_EDGE ( 'NONE', *, *, #5198, .T. ) ;
#2580 = CIRCLE ( 'NONE', #2, 7.983406227920510467 ) ;
#2581 = EDGE_CURVE ( 'NONE', #4723, #6208, #8803, .T. ) ;
#2582 = FILL_AREA_STYLE_COLOUR ( '', #12333 ) ;
#2583 = DIRECTION ( 'NONE',  ( -0.000000000000000000, -0.000000000000000000, 1.000000000000000000 ) ) ;
#2584 = CARTESIAN_POINT ( 'NONE',  ( 170.9999999999999716, 8.660254037844390851, 200.0000000000000000 ) ) ;
#2585 = SURFACE_SIDE_STYLE ('',( #444 ) ) ;
#2586 = ORIENTED_EDGE ( 'NONE', *, *, #11382, .F. ) ;
#2587 = VECTOR ( 'NONE', #2574, 1000.000000000000000 ) ;
#2588 = LINE ( 'NONE', #10564, #4334 ) ;
#2589 = EDGE_CURVE ( 'NONE', #10676, #2417, #9716, .T. ) ;
#2590 = ADVANCED_FACE ( 'NONE', ( #7705 ), #4308, .F. ) ;
#2591 = CARTESIAN_POINT ( 'NONE',  ( 1.799999999999996048, 0.000000000000000000, 0.000000000000000000 ) ) ;
#2592 = CARTESIAN_POINT ( 'NONE',  ( 264.0000000000000000, 0.000000000000000000, 0.000000000000000000 ) ) ;
#2593 = DIRECTION ( 'NONE',  ( 1.000000000000000000, 0.000000000000000000, 0.000000000000000000 ) ) ;
#2594 = ORIENTED_EDGE ( 'NONE', *, *, #1613, .T. ) ;
#2595 = EDGE_CURVE ( 'NONE', #11820, #7879, #3234, .T. ) ;
#2596 = CARTESIAN_POINT ( 'NONE',  ( -1.828356344711647319, -3.563200125723192002, -1.076197711133951296E-14 ) ) ;
#2597 = AXIS2_PLACEMENT_3D ( 'NONE', #4504, #11241, #10287 ) ;
#2598 = CARTESIAN_POINT ( 'NONE',  ( -124.9999999999999432, -65.00000000000008527, 30.00000000000000000 ) ) ;
#2599 = AXIS2_PLACEMENT_3D ( 'NONE', #9184, #10132, #8228 ) ;
#2600 = PRESENTATION_LAYER_ASSIGNMENT (  '', '', ( #8860 ) ) ;
#2601 = ORIENTED_EDGE ( 'NONE', *, *, #10191, .F. ) ;
#2602 = VERTEX_POINT ( 'NONE', #6621 ) ;
#2603 = CARTESIAN_POINT ( 'NONE',  ( -30.00000000000002842, -25.00000000000000000, 250.0000000000000000 ) ) ;
#2604 = CARTESIAN_POINT ( 'NONE',  ( -299.9999999999999432, -75.00000000000008527, 10.00000000000000178 ) ) ;
#2605 = CARTESIAN_POINT ( 'NONE',  ( 206.0000000000000284, -85.00000000000007105, 190.0000000000000000 ) ) ;
#2606 = EDGE_CURVE ( 'NONE', #4565, #7302, #10159, .T. ) ;
#2607 = DIRECTION ( 'NONE',  ( -0.000000000000000000, 1.000000000000000000, -0.000000000000000000 ) ) ;
#2608 = DIRECTION ( 'NONE',  ( 0.8660254037844374864, -0.5000000000000018874, 0.000000000000000000 ) ) ;
#2609 = DIRECTION ( 'NONE',  ( 1.000000000000000000, 0.000000000000000000, 0.000000000000000000 ) ) ;
#2610 = CIRCLE ( 'NONE', #12329, 7.983406227920510467 ) ;
#2611 = DIRECTION ( 'NONE',  ( 0.000000000000000000, 0.000000000000000000, 1.000000000000000000 ) ) ;
#2612 = ORIENTED_EDGE ( 'NONE', *, *, #13192, .F. ) ;
#2613 = EDGE_LOOP ( 'NONE', ( #438, #8269, #2615, #12189 ) ) ;
#2614 = AXIS2_PLACEMENT_3D ( 'NONE', #12834, #5163, #1726 ) ;
#2615 = ORIENTED_EDGE ( 'NONE', *, *, #10294, .T. ) ;
#2616 = EDGE_CURVE ( 'NONE', #13651, #6940, #10457, .T. ) ;
#2617 = DIRECTION ( 'NONE',  ( -0.000000000000000000, 1.000000000000000000, -0.000000000000000000 ) ) ;
#2618 = EDGE_LOOP ( 'NONE', ( #14249, #12035, #8287, #11770 ) ) ;
#2619 = LINE ( 'NONE', #10158, #7237 ) ;
#2620 = AXIS2_PLACEMENT_3D ( 'NONE', #3379, #8948, #7642 ) ;
#2621 = EDGE_CURVE ( 'NONE', #1904, #8368, #3907, .T. ) ;
#2622 = VERTEX_POINT ( 'NONE', #13561 ) ;
#2623 = CARTESIAN_POINT ( 'NONE',  ( 319.9999999999999432, -24.99999999999999289, -169.9999999999999716 ) ) ;
#2624 = VERTEX_POINT ( 'NONE', #8124 ) ;
#2625 = DIRECTION ( 'NONE',  ( 0.000000000000000000, -3.552713678800500929E-15, -1.000000000000000000 ) ) ;
#2626 = CARTESIAN_POINT ( 'NONE',  ( 5.200000000000002842, 0.000000000000000000, 0.000000000000000000 ) ) ;
#2627 = CARTESIAN_POINT ( 'NONE',  ( 297.3499999999999659, -95.00000000000008527, 186.2999999999999829 ) ) ;
#2628 = VERTEX_POINT ( 'NONE', #11474 ) ;
#2629 = DIRECTION ( 'NONE',  ( -0.000000000000000000, -0.000000000000000000, 1.000000000000000000 ) ) ;
#2630 = DIRECTION ( 'NONE',  ( 0.000000000000000000, 0.000000000000000000, 1.000000000000000000 ) ) ;
#2631 = SURFACE_STYLE_USAGE ( .BOTH. , #6030 ) ;
#2632 = FACE_BOUND ( 'NONE', #1888, .T. ) ;
#2633 = ORIENTED_EDGE ( 'NONE', *, *, #4794, .T. ) ;
#2634 = ORIENTED_EDGE ( 'NONE', *, *, #10400, .T. ) ;
#2635 = VERTEX_POINT ( 'NONE', #13638 ) ;
#2636 = FACE_BOUND ( 'NONE', #1805, .T. ) ;
#2637 = EDGE_CURVE ( 'NONE', #3406, #1151, #10240, .T. ) ;
#2638 = EDGE_LOOP ( 'NONE', ( #671, #5749, #13109, #891 ) ) ;
#2639 = FACE_OUTER_BOUND ( 'NONE', #3974, .T. ) ;
#2640 = ORIENTED_EDGE ( 'NONE', *, *, #1480, .T. ) ;
#2641 = CARTESIAN_POINT ( 'NONE',  ( 79.99999999999971578, 55.00000000000000711, 10.00000000000000000 ) ) ;
#2642 = CARTESIAN_POINT ( 'NONE',  ( 1.849560077140140812, 0.5149999999999973488, 0.7556913915602433418 ) ) ;
#2643 = CARTESIAN_POINT ( 'NONE',  ( 303.3333333333333144, -20.00000000000000000, -225.1500000000000625 ) ) ;
#2644 = CYLINDRICAL_SURFACE ( 'NONE', #8833, 4.749999999999999112 ) ;
#2645 = LINE ( 'NONE', #10327, #222 ) ;
#2646 = CARTESIAN_POINT ( 'NONE',  ( 0.000000000000000000, 0.000000000000000000, -5.000000000000000888 ) ) ;
#2647 = PRODUCT_DEFINITION_SHAPE ( 'NONE', 'NONE',  #14310 ) ;
#2648 = DIRECTION ( 'NONE',  ( 0.000000000000000000, 0.000000000000000000, 1.000000000000000000 ) ) ;
#2649 = ORIENTED_EDGE ( 'NONE', *, *, #4541, .T. ) ;
#2650 = DIRECTION ( 'NONE',  ( -0.000000000000000000, -0.000000000000000000, 1.000000000000000000 ) ) ;
#2651 = CARTESIAN_POINT ( 'NONE',  ( 137.3500000000000227, -95.00000000000008527, -169.9999999999999716 ) ) ;
#2652 = DIRECTION ( 'NONE',  ( -0.8191520442889902442, 0.000000000000000000, -0.5735764363510482688 ) ) ;
#2653 = EDGE_LOOP ( 'NONE', ( #10031, #6056, #2509, #8651 ) ) ;
#2654 = CYLINDRICAL_SURFACE ( 'NONE', #2353, 2.649999999999985700 ) ;
#2655 = EDGE_CURVE ( 'NONE', #1332, #9383, #10399, .T. ) ;
#2656 = LINE ( 'NONE', #11367, #6007 ) ;
#2657 = CARTESIAN_POINT ( 'NONE',  ( 53.33333333333330017, -30.00000000000000355, -222.5000000000000853 ) ) ;
#2658 = EDGE_CURVE ( 'NONE', #3958, #4926, #9300, .T. ) ;
#2659 = DIRECTION ( 'NONE',  ( 0.000000000000000000, 1.000000000000000000, 0.000000000000000000 ) ) ;
#2660 =( REPRESENTATION_RELATIONSHIP ('NONE','NONE', #11251, #13104 ) REPRESENTATION_RELATIONSHIP_WITH_TRANSFORMATION ( #8489 )SHAPE_REPRESENTATION_RELATIONSHIP( ) );
#2661 = CIRCLE ( 'NONE', #6836, 10.72499999999999964 ) ;
#2662 = ORIENTED_EDGE ( 'NONE', *, *, #7023, .F. ) ;
#2663 = FACE_OUTER_BOUND ( 'NONE', #1603, .T. ) ;
#2664 = LINE ( 'NONE', #5858, #6505 ) ;
#2665 = VERTEX_POINT ( 'NONE', #488 ) ;
#2666 = DIRECTION ( 'NONE',  ( 0.000000000000000000, 0.000000000000000000, 1.000000000000000000 ) ) ;
#2667 = FACE_OUTER_BOUND ( 'NONE', #3289, .T. ) ;
#2668 = VECTOR ( 'NONE', #5368, 1000.000000000000000 ) ;
#2669 = FACE_OUTER_BOUND ( 'NONE', #513, .T. ) ;
#2670 = EDGE_CURVE ( 'NONE', #4036, #2471, #4699, .T. ) ;
#2671 = CARTESIAN_POINT ( 'NONE',  ( 137.3500000000000227, -95.00000000000008527, 190.0000000000000000 ) ) ;
#2672 = EDGE_CURVE ( 'NONE', #2854, #6402, #2053, .T. ) ;
#2673 = CARTESIAN_POINT ( 'NONE',  ( -2.687328764639638656, 3.067272167851286202, -0.05923475698270370959 ) ) ;
#2674 = DIRECTION ( 'NONE',  ( -0.000000000000000000, -0.000000000000000000, 1.000000000000000000 ) ) ;
#2675 = CARTESIAN_POINT ( 'NONE',  ( 203.5000000000000000, -85.00000000000007105, 190.0000000000000000 ) ) ;
#2676 = CONTEXT_DEPENDENT_SHAPE_REPRESENTATION ( #6224, #6000 ) ;
#2677 = VERTEX_POINT ( 'NONE', #12412 ) ;
#2678 = EDGE_CURVE ( 'NONE', #9294, #7034, #4737, .T. ) ;
#2679 = ORIENTED_EDGE ( 'NONE', *, *, #12960, .F. ) ;
#2680 = FACE_OUTER_BOUND ( 'NONE', #6752, .T. ) ;
#2681 = AXIS2_PLACEMENT_3D ( 'NONE', #5396, #4305, #8657 ) ;
#2682 = ORIENTED_EDGE ( 'NONE', *, *, #1154, .T. ) ;
#2683 = CARTESIAN_POINT ( 'NONE',  ( 4.211140560182196957, -2.431303136016555122, -3.745885042887436622 ) ) ;
#2684 = DIRECTION ( 'NONE',  ( -0.000000000000000000, -0.000000000000000000, 1.000000000000000000 ) ) ;
#2685 = ADVANCED_FACE ( 'NONE', ( #5816 ), #7045, .F. ) ;
#2686 = ADVANCED_FACE ( 'NONE', ( #2481 ), #12625, .T. ) ;
#2687 = VERTEX_POINT ( 'NONE', #1378 ) ;
#2688 = ADVANCED_FACE ( 'NONE', ( #11544 ), #10169, .F. ) ;
#2689 = DIRECTION ( 'NONE',  ( -1.000000000000000000, 0.000000000000000000, 0.000000000000000000 ) ) ;
#2690 = ORIENTED_EDGE ( 'NONE', *, *, #5877, .T. ) ;
#2691 = ADVANCED_FACE ( 'NONE', ( #3640 ), #12349, .T. ) ;
#2692 = FACE_OUTER_BOUND ( 'NONE', #10415, .T. ) ;
#2693 = CARTESIAN_POINT ( 'NONE',  ( 222.0549999999999216, -85.00000000000009948, -18.00000000000000355 ) ) ;
#2694 = ORIENTED_EDGE ( 'NONE', *, *, #9241, .T. ) ;
#2695 = LINE ( 'NONE', #11472, #7591 ) ;
#2696 = ADVANCED_FACE ( 'NONE', ( #9148 ), #3572, .F. ) ;
#2697 = DIRECTION ( 'NONE',  ( -1.000000000000000000, 0.000000000000000000, 0.000000000000000000 ) ) ;
#2698 = AXIS2_PLACEMENT_3D ( 'NONE', #773, #5233, #7677 ) ;
#2699 = FILL_AREA_STYLE_COLOUR ( '', #13726 ) ;
#2700 = CARTESIAN_POINT ( 'NONE',  ( 219.9999999999999716, -85.00000000000007105, 190.0000000000000000 ) ) ;
#2701 = APPLICATION_PROTOCOL_DEFINITION ( 'draft international standard', 'automotive_design', 1998, #9055 ) ;
#2702 = AXIS2_PLACEMENT_3D ( 'NONE', #7505, #7288, #12947 ) ;
#2703 = ORIENTED_EDGE ( 'NONE', *, *, #3672, .T. ) ;
#2704 = ORIENTED_EDGE ( 'NONE', *, *, #8884, .T. ) ;
#2705 = AXIS2_PLACEMENT_3D ( 'NONE', #8929, #11660, #604 ) ;
#2706 = EDGE_LOOP ( 'NONE', ( #9877, #11737, #6542, #7671 ) ) ;
#2707 = CARTESIAN_POINT ( 'NONE',  ( -294.9999999999999432, -105.0000000000000853, 40.00000000000000000 ) ) ;
#2708 = AXIS2_PLACEMENT_3D ( 'NONE', #12749, #5932, #9276 ) ;
#2709 = VECTOR ( 'NONE', #2970, 1000.000000000000000 ) ;
#2710 = VERTEX_POINT ( 'NONE', #5888 ) ;
#2711 = DIRECTION ( 'NONE',  ( 1.000000000000000000, 0.000000000000000000, 0.000000000000000000 ) ) ;
#2712 = ORIENTED_EDGE ( 'NONE', *, *, #6511, .T. ) ;
#2713 = LINE ( 'NONE', #13796, #2012 ) ;
#2714 = VECTOR ( 'NONE', #8375, 1000.000000000000000 ) ;
#2715 = DIRECTION ( 'NONE',  ( -0.000000000000000000, -0.000000000000000000, 1.000000000000000000 ) ) ;
#2716 = FACE_BOUND ( 'NONE', #8671, .T. ) ;
#2717 = AXIS2_PLACEMENT_3D ( 'NONE', #1683, #4894, #13871 ) ;
#2718 = DIRECTION ( 'NONE',  ( 0.000000000000000000, 0.000000000000000000, -1.000000000000000000 ) ) ;
#2719 = DIRECTION ( 'NONE',  ( -0.000000000000000000, -0.000000000000000000, 1.000000000000000000 ) ) ;
#2720 = PRESENTATION_LAYER_ASSIGNMENT (  '', '', ( #1314 ) ) ;
#2721 = CYLINDRICAL_SURFACE ( 'NONE', #2991, 2.649999999999985700 ) ;
#2722 = ORIENTED_EDGE ( 'NONE', *, *, #4726, .T. ) ;
#2723 = EDGE_CURVE ( 'NONE', #2940, #13395, #1386, .T. ) ;
#2724 = AXIS2_PLACEMENT_3D ( 'NONE', #14154, #8655, #13869 ) ;
#2725 = ORIENTED_EDGE ( 'NONE', *, *, #693, .F. ) ;
#2726 = AXIS2_PLACEMENT_3D ( 'NONE', #2194, #8872, #12134 ) ;
#2727 = SHAPE_REPRESENTATION_RELATIONSHIP ( 'NONE' , 'NONE' ,  #11637, #1054 ) ;
#2728 = CIRCLE ( 'NONE', #8975, 2.649999999999985700 ) ;
#2729 = CARTESIAN_POINT ( 'NONE',  ( 119.9999999999999147, -20.00000000000000000, -19.99999999999998934 ) ) ;
#2730 = DIRECTION ( 'NONE',  ( 1.000000000000000000, 0.000000000000000000, 0.000000000000000000 ) ) ;
#2731 = CIRCLE ( 'NONE', #14297, 2.649999999999985700 ) ;
#2732 = CARTESIAN_POINT ( 'NONE',  ( 2.500000000000000000, -2.357898499370432610, 3.252606517456513302E-15 ) ) ;
#2733 = ORIENTED_EDGE ( 'NONE', *, *, #9631, .T. ) ;
#2734 = VECTOR ( 'NONE', #11680, 1000.000000000000000 ) ;
#2735 = FACE_OUTER_BOUND ( 'NONE', #1758, .T. ) ;
#2736 = PLANE ( 'NONE',  #418 ) ;
#2737 = CARTESIAN_POINT ( 'NONE',  ( 439.9999999999999432, 0.000000000000000000, 188.0000000000000000 ) ) ;
#2738 = LINE ( 'NONE', #13818, #8565 ) ;
#2739 = DIRECTION ( 'NONE',  ( -0.000000000000000000, 0.000000000000000000, 1.000000000000000000 ) ) ;
#2740 = SHAPE_REPRESENTATION ( 'base table', ( #14039 ), #7000 ) ;
#2741 = VERTEX_POINT ( 'NONE', #13500 ) ;
#2742 = VECTOR ( 'NONE', #3889, 1000.000000000000000 ) ;
#2743 = DIRECTION ( 'NONE',  ( -0.000000000000000000, -0.000000000000000000, 1.000000000000000000 ) ) ;
#2744 = FACE_BOUND ( 'NONE', #5201, .T. ) ;
#2745 = ADVANCED_FACE ( 'NONE', ( #7407 ), #7327, .F. ) ;
#2746 = VERTEX_POINT ( 'NONE', #1665 ) ;
#2747 = DIRECTION ( 'NONE',  ( 0.000000000000000000, 0.000000000000000000, -1.000000000000000000 ) ) ;
#2748 = CARTESIAN_POINT ( 'NONE',  ( 3.900000000000000799, 0.000000000000000000, 2.700000000000000178 ) ) ;
#2749 = CARTESIAN_POINT ( 'NONE',  ( 0.000000000000000000, 1.178949249685217415, 2.041999999999998483 ) ) ;
#2750 = CARTESIAN_POINT ( 'NONE',  ( 134.9999999999999432, -36.99999999999997868, -169.9999999999999716 ) ) ;
#2751 = CARTESIAN_POINT ( 'NONE',  ( -3.455068668934486276, 2.624017327439035707, -3.316620875263955437 ) ) ;
#2752 = CIRCLE ( 'NONE', #8074, 5.500000000000005329 ) ;
#2753 = ORIENTED_EDGE ( 'NONE', *, *, #11673, .T. ) ;
#2754 = DIRECTION ( 'NONE',  ( -1.000000000000000000, -0.000000000000000000, -0.000000000000000000 ) ) ;
#2755 = ORIENTED_EDGE ( 'NONE', *, *, #4202, .T. ) ;
#2756 = CARTESIAN_POINT ( 'NONE',  ( 170.9999999999999716, 8.660254037844390851, 199.9990000000000236 ) ) ;
#2757 = CARTESIAN_POINT ( 'NONE',  ( 0.2277608394786177770, 0.000000000000000000, 0.000000000000000000 ) ) ;
#2758 = EDGE_CURVE ( 'NONE', #9311, #4062, #10893, .T. ) ;
#2759 = ORIENTED_EDGE ( 'NONE', *, *, #3672, .F. ) ;
#2760 = CARTESIAN_POINT ( 'NONE',  ( -0.3461262719736137305, 4.658553426539289610, -3.671615880910373608 ) ) ;
#2761 = ORIENTED_EDGE ( 'NONE', *, *, #1527, .F. ) ;
#2762 = AXIS2_PLACEMENT_3D ( 'NONE', #165, #236, #13458 ) ;
#2763 = CARTESIAN_POINT ( 'NONE',  ( 0.06760930072668894231, 0.9010842325122760954, 0.5149999999999993472 ) ) ;
#2764 = PRODUCT_DEFINITION_SHAPE ( 'NONE', 'NONE',  #14339 ) ;
#2765 = DIRECTION ( 'NONE',  ( 0.000000000000000000, 0.000000000000000000, -1.000000000000000000 ) ) ;
#2766 = VERTEX_POINT ( 'NONE', #6246 ) ;
#2767 = PRODUCT_DEFINITION_CONTEXT ( 'detailed design', #12304, 'design' ) ;
#2768 = CARTESIAN_POINT ( 'NONE',  ( -30.00000000000002842, -25.00000000000000000, 250.0000000000000000 ) ) ;
#2769 = DIRECTION ( 'NONE',  ( -1.000000000000000000, 0.000000000000000000, 0.000000000000000000 ) ) ;
#2770 = SHAPE_REPRESENTATION_RELATIONSHIP ( 'NONE' , 'NONE' ,  #9307, #12151 ) ;
#2771 = DIRECTION ( 'NONE',  ( -1.000000000000000000, 0.000000000000000000, 0.000000000000000000 ) ) ;
#2772 = APPLICATION_PROTOCOL_DEFINITION ( 'draft international standard', 'automotive_design', 1998, #5364 ) ;
#2773 = EDGE_CURVE ( 'NONE', #1006, #1448, #8637, .T. ) ;
#2774 = ADVANCED_FACE ( 'NONE', ( #6391 ), #9734, .F. ) ;
#2775 = CARTESIAN_POINT ( 'NONE',  ( -0.6666666666666651864, 4.233901974057260098, -3.300726591567081147 ) ) ;
#2776 = ORIENTED_EDGE ( 'NONE', *, *, #10321, .T. ) ;
#2777 = EDGE_CURVE ( 'NONE', #7324, #3696, #11882, .T. ) ;
#2778 = AXIS2_PLACEMENT_3D ( 'NONE', #2429, #10406, #435 ) ;
#2779 = ORIENTED_EDGE ( 'NONE', *, *, #6667, .T. ) ;
#2780 = ORIENTED_EDGE ( 'NONE', *, *, #12164, .F. ) ;
#2781 = ORIENTED_EDGE ( 'NONE', *, *, #5876, .F. ) ;
#2782 = VECTOR ( 'NONE', #11727, 1000.000000000000000 ) ;
#2783 = CARTESIAN_POINT ( 'NONE',  ( -13.50000000000000000, 0.000000000000000000, -186.0000000000000000 ) ) ;
#2784 = ORIENTED_EDGE ( 'NONE', *, *, #3663, .T. ) ;
#2785 = DIRECTION ( 'NONE',  ( 0.000000000000000000, 0.000000000000000000, 1.000000000000000000 ) ) ;
#2786 = EDGE_LOOP ( 'NONE', ( #13164, #6145 ) ) ;
#2787 = PLANE ( 'NONE',  #9424 ) ;
#2788 = CARTESIAN_POINT ( 'NONE',  ( 4.197393957002303999, 7.772902908466098641E-14, -3.503767560748929810 ) ) ;
#2789 = CARTESIAN_POINT ( 'NONE',  ( 2.500000000000000000, -1.178949249685213863, 2.042000000000002924 ) ) ;
#2790 = DIRECTION ( 'NONE',  ( 0.000000000000000000, 0.000000000000000000, 1.000000000000000000 ) ) ;
#2791 = VECTOR ( 'NONE', #2154, 1000.000000000000000 ) ;
#2792 = VECTOR ( 'NONE', #10884, 1000.000000000000000 ) ;
#2793 = DIRECTION ( 'NONE',  ( -0.000000000000000000, -0.000000000000000000, -1.000000000000000000 ) ) ;
#2794 = CARTESIAN_POINT ( 'NONE',  ( -13.50000000000000000, 0.000000000000000000, -190.0000000000000000 ) ) ;
#2795 = ADVANCED_FACE ( 'NONE', ( #6173 ), #4070, .F. ) ;
#2796 = ORIENTED_EDGE ( 'NONE', *, *, #3663, .F. ) ;
#2797 = ORIENTED_EDGE ( 'NONE', *, *, #9345, .F. ) ;
#2798 = PLANE ( 'NONE',  #9100 ) ;
#2799 = AXIS2_PLACEMENT_3D ( 'NONE', #12668, #3686, #10575 ) ;
#2800 =( REPRESENTATION_RELATIONSHIP ('NONE','NONE', #11251, #9307 ) REPRESENTATION_RELATIONSHIP_WITH_TRANSFORMATION ( #13767 )SHAPE_REPRESENTATION_RELATIONSHIP( ) );
#2801 = ORIENTED_EDGE ( 'NONE', *, *, #4387, .T. ) ;
#2802 = FACE_OUTER_BOUND ( 'NONE', #1531, .T. ) ;
#2803 = CARTESIAN_POINT ( 'NONE',  ( 0.06760930072668894231, -0.9010842325122859764, 0.5149999999999992362 ) ) ;
#2804 =( NAMED_UNIT ( * ) SI_UNIT ( $, .STERADIAN. ) SOLID_ANGLE_UNIT ( ) );
#2805 = ORIENTED_EDGE ( 'NONE', *, *, #11204, .F. ) ;
#2806 = AXIS2_PLACEMENT_3D ( 'NONE', #7241, #3831, #12678 ) ;
#2807 = CARTESIAN_POINT ( 'NONE',  ( 2.500000000000000000, 2.357898499370433054, -1.951563910473907981E-15 ) ) ;
#2808 = CARTESIAN_POINT ( 'NONE',  ( -299.9999999999999432, -75.00000000000008527, 339.9999999999999432 ) ) ;
#2809 = DIRECTION ( 'NONE',  ( 0.000000000000000000, 0.000000000000000000, -1.000000000000000000 ) ) ;
#2810 = VECTOR ( 'NONE', #7862, 1000.000000000000000 ) ;
#2811 = CARTESIAN_POINT ( 'NONE',  ( 469.9999999999998863, -225.0000000000000000, -190.0000000000000000 ) ) ;
#2812 = CARTESIAN_POINT ( 'NONE',  ( 259.0000000000000000, 8.660254037844390851, 205.0000000000000284 ) ) ;
#2813 = CONICAL_SURFACE ( 'NONE', #5584, 2.500000000000002220, 1.029744260000002631 ) ;
#2814 = VERTEX_POINT ( 'NONE', #7260 ) ;
#2815 = CARTESIAN_POINT ( 'NONE',  ( 444.9999999999999432, 8.660254037844390851, 200.0000000000000000 ) ) ;
#2816 = DIRECTION ( 'NONE',  ( 0.000000000000000000, -1.000000000000000000, 0.000000000000000000 ) ) ;
#2817 = AXIS2_PLACEMENT_3D ( 'NONE', #1926, #8379, #11945 ) ;
#2818 = EDGE_CURVE ( 'NONE', #1984, #1298, #6785, .T. ) ;
#2819 = ORIENTED_EDGE ( 'NONE', *, *, #2883, .F. ) ;
#2820 = CARTESIAN_POINT ( 'NONE',  ( 1.999999999999998224, 0.000000000000000000, 0.000000000000000000 ) ) ;
#2821 = MECHANICAL_DESIGN_GEOMETRIC_PRESENTATION_REPRESENTATION (  '', ( #8373 ), #1652 ) ;
#2822 =( NAMED_UNIT ( * ) PLANE_ANGLE_UNIT ( ) SI_UNIT ( $, .RADIAN. ) );
#2823 = SURFACE_STYLE_USAGE ( .BOTH. , #12677 ) ;
#2824 = FACE_OUTER_BOUND ( 'NONE', #13768, .T. ) ;
#2825 = CARTESIAN_POINT ( 'NONE',  ( 0.000000000000000000, 0.000000000000000000, -200.0000000000000000 ) ) ;
#2826 = CARTESIAN_POINT ( 'NONE',  ( 5.200000000000002842, 3.306546357697854719E-16, 2.700000000000001066 ) ) ;
#2827 = CARTESIAN_POINT ( 'NONE',  ( 3.999999999999999112, 1.941961291383486277, -0.3515519931180248192 ) ) ;
#2828 = CIRCLE ( 'NONE', #10943, 2.500000000000002220 ) ;
#2829 = ORIENTED_EDGE ( 'NONE', *, *, #6117, .T. ) ;
#2830 = DIRECTION ( 'NONE',  ( 0.000000000000000000, 0.000000000000000000, -1.000000000000000000 ) ) ;
#2831 = AXIS2_PLACEMENT_3D ( 'NONE', #11579, #237, #3815 ) ;
#2832 = ORIENTED_EDGE ( 'NONE', *, *, #13056, .F. ) ;
#2833 = VECTOR ( 'NONE', #3291, 1000.000000000000000 ) ;
#2834 = CARTESIAN_POINT ( 'NONE',  ( 386.6666666666666288, -25.00000000000000000, 219.8500000000001080 ) ) ;
#2835 = DIRECTION ( 'NONE',  ( -0.000000000000000000, -0.000000000000000000, -1.000000000000000000 ) ) ;
#2836 = EDGE_LOOP ( 'NONE', ( #13020, #830, #4442, #5052 ) ) ;
#2837 = CARTESIAN_POINT ( 'NONE',  ( 242.5000000000000000, -90.00000000000007105, 50.00000000000001421 ) ) ;
#2838 = VERTEX_POINT ( 'NONE', #10680 ) ;
#2839 = FACE_OUTER_BOUND ( 'NONE', #4330, .T. ) ;
#2840 = FACE_OUTER_BOUND ( 'NONE', #7947, .T. ) ;
#2842 = VERTEX_POINT ( 'NONE', #2844 ) ;
#2841 = AXIS2_PLACEMENT_3D ( 'NONE', #9331, #11649, #9547 ) ;
#2843 = DIRECTION ( 'NONE',  ( -1.000000000000000000, 0.000000000000000000, 0.000000000000000000 ) ) ;
#2844 = CARTESIAN_POINT ( 'NONE',  ( 303.3333333333333144, -14.99999999999999822, 225.1500000000000625 ) ) ;
#2845 = ORIENTED_EDGE ( 'NONE', *, *, #940, .T. ) ;
#2846 =( NAMED_UNIT ( * ) PLANE_ANGLE_UNIT ( ) SI_UNIT ( $, .RADIAN. ) );
#2847 =( GEOMETRIC_REPRESENTATION_CONTEXT ( 3 ) GLOBAL_UNCERTAINTY_ASSIGNED_CONTEXT ( ( #8575 ) ) GLOBAL_UNIT_ASSIGNED_CONTEXT ( ( #1091, #11261, #1205 ) ) REPRESENTATION_CONTEXT ( 'NONE', 'WORKASPACE' ) );
#2848 = ADVANCED_FACE ( 'NONE', ( #709 ), #12919, .F. ) ;
#2849 = SHAPE_DEFINITION_REPRESENTATION ( #7724, #3832 ) ;
#2850 = DIRECTION ( 'NONE',  ( 0.000000000000000000, 1.000000000000000000, 0.000000000000000000 ) ) ;
#2851 = EDGE_CURVE ( 'NONE', #2569, #10145, #1676, .T. ) ;
#2852 = ORIENTED_EDGE ( 'NONE', *, *, #11, .F. ) ;
#2853 = ORIENTED_EDGE ( 'NONE', *, *, #2513, .F. ) ;
#2854 = VERTEX_POINT ( 'NONE', #641 ) ;
#2855 = AXIS2_PLACEMENT_3D ( 'NONE', #11790, #3957, #5129 ) ;
#2856 = ORIENTED_EDGE ( 'NONE', *, *, #11438, .F. ) ;
#2857 = CARTESIAN_POINT ( 'NONE',  ( 2.855764796983346177, -2.970025579236428737, -0.09382832055446485575 ) ) ;
#2858 = DIRECTION ( 'NONE',  ( 1.000000000000000000, 0.000000000000000000, 0.000000000000000000 ) ) ;
#2859 = ORIENTED_EDGE ( 'NONE', *, *, #3725, .T. ) ;
#2860 = LINE ( 'NONE', #7697, #1070 ) ;
#2861 = VERTEX_POINT ( 'NONE', #9660 ) ;
#2862 = CYLINDRICAL_SURFACE ( 'NONE', #13359, 13.50000000000000000 ) ;
#2863 = ADVANCED_FACE ( 'NONE', ( #1736 ), #4146, .T. ) ;
#2864 = UNCERTAINTY_MEASURE_WITH_UNIT (LENGTH_MEASURE( 1.000000000000000082E-05 ), #10947, 'distance_accuracy_value', 'NONE');
#2865 = CARTESIAN_POINT ( 'NONE',  ( 2.500000000000000000, 2.357898499370433054, -1.951563910473907981E-15 ) ) ;
#2866 = DIRECTION ( 'NONE',  ( 0.000000000000000000, 0.000000000000000000, -1.000000000000000000 ) ) ;
#2867 =( REPRESENTATION_RELATIONSHIP ('NONE','NONE', #11251, #13104 ) REPRESENTATION_RELATIONSHIP_WITH_TRANSFORMATION ( #14143 )SHAPE_REPRESENTATION_RELATIONSHIP( ) );
#2868 = DIRECTION ( 'NONE',  ( -0.000000000000000000, 1.000000000000000000, -0.000000000000000000 ) ) ;
#2869 = DIRECTION ( 'NONE',  ( -1.000000000000000000, 0.000000000000000000, 0.000000000000000000 ) ) ;
#2870 = EDGE_CURVE ( 'NONE', #8841, #8377, #854, .T. ) ;
#2871 = DIRECTION ( 'NONE',  ( 0.000000000000000000, 0.000000000000000000, 1.000000000000000000 ) ) ;
#2872 = VERTEX_POINT ( 'NONE', #12699 ) ;
#2873 = EDGE_LOOP ( 'NONE', ( #3414, #9238, #9236, #1813 ) ) ;
#2874 = CARTESIAN_POINT ( 'NONE',  ( -4.000000000000000000, -2.309401076758512694, -3.433295621305382461 ) ) ;
#2875 = ORIENTED_EDGE ( 'NONE', *, *, #7194, .T. ) ;
#2876 = LINE ( 'NONE', #9695, #5702 ) ;
#2877 = DIRECTION ( 'NONE',  ( 1.000000000000000000, 0.000000000000000000, 0.000000000000000000 ) ) ;
#2878 = EDGE_CURVE ( 'NONE', #1188, #10103, #3668, .T. ) ;
#2879 = DIRECTION ( 'NONE',  ( -1.000000000000000000, 0.000000000000000000, 0.000000000000000000 ) ) ;
#2880 = ORIENTED_EDGE ( 'NONE', *, *, #8265, .T. ) ;
#2881 = EDGE_CURVE ( 'NONE', #764, #7188, #7370, .T. ) ;
#2882 = PLANE ( 'NONE',  #4905 ) ;
#2883 = EDGE_CURVE ( 'NONE', #1770, #10068, #9446, .T. ) ;
#2884 = DIRECTION ( 'NONE',  ( 0.000000000000000000, 0.000000000000000000, -1.000000000000000000 ) ) ;
#2885 = CARTESIAN_POINT ( 'NONE',  ( 303.3333333333333144, -30.00000000000000355, -222.5000000000000853 ) ) ;
#2886 = DIRECTION ( 'NONE',  ( 1.000000000000000000, 0.000000000000000000, 0.000000000000000000 ) ) ;
#2887 = VERTEX_POINT ( 'NONE', #5103 ) ;
#2888 = DIRECTION ( 'NONE',  ( -0.000000000000000000, 0.000000000000000000, 1.000000000000000000 ) ) ;
#2889 = PRODUCT_DEFINITION_SHAPE ( 'NONE', 'NONE',  #14351 ) ;
#2890 = CARTESIAN_POINT ( 'NONE',  ( 229.9999999999999716, -85.00000000000007105, 169.9999999999999716 ) ) ;
#2891 = ORIENTED_EDGE ( 'NONE', *, *, #7963, .T. ) ;
#2892 = DIRECTION ( 'NONE',  ( -1.000000000000000000, 0.000000000000000000, 0.000000000000000000 ) ) ;
#2893 = DIRECTION ( 'NONE',  ( -1.000000000000000000, 0.000000000000000000, 0.000000000000000000 ) ) ;
#2894 = CYLINDRICAL_SURFACE ( 'NONE', #4649, 2.649999999999985700 ) ;
#2895 = LINE ( 'NONE', #9572, #2533 ) ;
#2896 =( LENGTH_UNIT ( ) NAMED_UNIT ( * ) SI_UNIT ( .MILLI., .METRE. ) );
#2897 = CIRCLE ( 'NONE', #6822, 1.050000000000000488 ) ;
#2898 = CARTESIAN_POINT ( 'NONE',  ( 4.000000000000000000, 0.7924765000094659007, -0.05906175389889852662 ) ) ;
#2899 = CONTEXT_DEPENDENT_SHAPE_REPRESENTATION ( #1015, #5099 ) ;
#2900 = ADVANCED_FACE ( 'NONE', ( #4000 ), #5585, .F. ) ;
#2901 = ORIENTED_EDGE ( 'NONE', *, *, #5908, .F. ) ;
#2902 = CARTESIAN_POINT ( 'NONE',  ( 119.9999999999999147, -225.0010000000000048, 19.99999999999998934 ) ) ;
#2903 = ORIENTED_EDGE ( 'NONE', *, *, #9861, .F. ) ;
#2904 = LINE ( 'NONE', #11533, #13046 ) ;
#2905 = CARTESIAN_POINT ( 'NONE',  ( -222.6499999999998920, -85.00000000000009948, 30.00000000000000000 ) ) ;
#2906 = AXIS2_PLACEMENT_3D ( 'NONE', #13308, #14109, #6503 ) ;
#2907 = VERTEX_POINT ( 'NONE', #6677 ) ;
#2908 = CARTESIAN_POINT ( 'NONE',  ( -299.9999999999999432, -75.00000000000008527, 0.000000000000000000 ) ) ;
#2909 = EDGE_LOOP ( 'NONE', ( #12132, #1459, #6840, #3447 ) ) ;
#2910 = CARTESIAN_POINT ( 'NONE',  ( -20.00000000000000000, 0.000000000000000000, -190.0000000000000000 ) ) ;
#2911 = DIRECTION ( 'NONE',  ( 0.000000000000000000, 0.000000000000000000, 1.000000000000000000 ) ) ;
#2912 = ORIENTED_EDGE ( 'NONE', *, *, #12783, .T. ) ;
#2913 = FILL_AREA_STYLE_COLOUR ( '', #5279 ) ;
#2914 = DIRECTION ( 'NONE',  ( -0.000000000000000000, -1.000000000000000000, -0.000000000000000000 ) ) ;
#2915 = CYLINDRICAL_SURFACE ( 'NONE', #14123, 5.500000000000005329 ) ;
#2916 = CARTESIAN_POINT ( 'NONE',  ( 444.9999999999999432, -8.660254037844389075, 205.0000000000000284 ) ) ;
#2917 = VECTOR ( 'NONE', #10839, 1000.000000000000000 ) ;
#2918 = EDGE_CURVE ( 'NONE', #1381, #2563, #7751, .T. ) ;
#2919 = VERTEX_POINT ( 'NONE', #4503 ) ;
#2920 = VECTOR ( 'NONE', #7945, 1000.000000000000000 ) ;
#2921 = ORIENTED_EDGE ( 'NONE', *, *, #14198, .F. ) ;
#2922 = ORIENTED_EDGE ( 'NONE', *, *, #980, .T. ) ;
#2923 = B_SPLINE_CURVE_WITH_KNOTS ( 'NONE', 3,
 ( #12118, #4603, #6779, #7644, #12081, #4398 ),
 .UNSPECIFIED., .F., .F.,
 ( 4, 2, 4 ),
 ( 0.002365888236228001588, 0.003551327329835089319, 0.004736766423442177049 ),
 .UNSPECIFIED. ) ;
#2924 = VERTEX_POINT ( 'NONE', #11035 ) ;
#2925 = CARTESIAN_POINT ( 'NONE',  ( -5.000000000000000888, 8.660254037844390851, 200.0000000000000000 ) ) ;
#2926 = ORIENTED_EDGE ( 'NONE', *, *, #12474, .T. ) ;
#2927 = FACE_OUTER_BOUND ( 'NONE', #11134, .T. ) ;
#2928 = VERTEX_POINT ( 'NONE', #8641 ) ;
#2929 = EDGE_CURVE ( 'NONE', #12902, #12884, #177, .T. ) ;
#2930 = FACE_BOUND ( 'NONE', #10179, .T. ) ;
#2931 = AXIS2_PLACEMENT_3D ( 'NONE', #7474, #14068, #9653 ) ;
#2932 = DIRECTION ( 'NONE',  ( -0.000000000000000000, -0.000000000000000000, -1.000000000000000000 ) ) ;
#2933 = CARTESIAN_POINT ( 'NONE',  ( 0.2500000000000002220, 0.000000000000000000, 0.000000000000000000 ) ) ;
#2934 = TOROIDAL_SURFACE ( 'NONE', #4779, 13.29999999999999893, 0.2000000000000027034 ) ;
#2935 = DIRECTION ( 'NONE',  ( 0.000000000000000000, 0.000000000000000000, -1.000000000000000000 ) ) ;
#2936 = FACE_OUTER_BOUND ( 'NONE', #6178, .T. ) ;
#2937 = AXIS2_PLACEMENT_3D ( 'NONE', #7015, #13605, #9186 ) ;
#2938 = ORIENTED_EDGE ( 'NONE', *, *, #12515, .F. ) ;
#2939 = VECTOR ( 'NONE', #7088, 1000.000000000000000 ) ;
#2940 = VERTEX_POINT ( 'NONE', #14280 ) ;
#2941 = CIRCLE ( 'NONE', #6174, 2.649999999999985700 ) ;
#2943 = DIRECTION ( 'NONE',  ( -0.000000000000000000, 1.471414886128461471E-15, 1.000000000000000000 ) ) ;
#2942 = CIRCLE ( 'NONE', #3179, 5.000000000000004441 ) ;
#2944 = ORIENTED_EDGE ( 'NONE', *, *, #6357, .T. ) ;
#2945 = CARTESIAN_POINT ( 'NONE',  ( 181.0000000000000000, 8.660254037844390851, 205.0000000000000284 ) ) ;
#2946 = EDGE_CURVE ( 'NONE', #7986, #7291, #3916, .T. ) ;
#2947 = DIRECTION ( 'NONE',  ( -0.000000000000000000, -0.000000000000000000, 1.000000000000000000 ) ) ;
#2948 = ADVANCED_FACE ( 'NONE', ( #4364 ), #8706, .T. ) ;
#2949 = CARTESIAN_POINT ( 'NONE',  ( -144.9999999999999432, -65.00000000000008527, 40.00000000000000000 ) ) ;
#2950 = VECTOR ( 'NONE', #254, 1000.000000000000000 ) ;
#2951 = ORIENTED_EDGE ( 'NONE', *, *, #5553, .F. ) ;
#2952 = VECTOR ( 'NONE', #10305, 1000.000000000000000 ) ;
#2953 = PLANE ( 'NONE',  #5825 ) ;
#2954 = CIRCLE ( 'NONE', #11066, 10.00000000000000000 ) ;
#2955 = CARTESIAN_POINT ( 'NONE',  ( -31.74999999999995737, 0.000000000000000000, 0.000000000000000000 ) ) ;
#2956 = DIRECTION ( 'NONE',  ( 2.822645452655844899E-19, -3.948310598970913925E-18, -1.000000000000000000 ) ) ;
#2957 = VECTOR ( 'NONE', #11401, 1000.000000000000114 ) ;
#2958 = CARTESIAN_POINT ( 'NONE',  ( -30.00000000000002842, -25.00000000000000000, -250.0000000000000000 ) ) ;
#2959 = EDGE_CURVE ( 'NONE', #5706, #1098, #4613, .T. ) ;
#2960 = EDGE_CURVE ( 'NONE', #2417, #12823, #2247, .T. ) ;
#2961 = ORIENTED_EDGE ( 'NONE', *, *, #3232, .T. ) ;
#2962 = AXIS2_PLACEMENT_3D ( 'NONE', #13079, #9970, #11131 ) ;
#2963 = EDGE_CURVE ( 'NONE', #10177, #10192, #1139, .T. ) ;
#2964 = ORIENTED_EDGE ( 'NONE', *, *, #900, .F. ) ;
#2965 = DIRECTION ( 'NONE',  ( 1.000000000000000000, 0.000000000000000000, -0.000000000000000000 ) ) ;
#2966 = CIRCLE ( 'NONE', #8977, 10.00000000000000888 ) ;
#2967 = DIRECTION ( 'NONE',  ( -1.000000000000000000, -0.000000000000000000, -0.000000000000000000 ) ) ;
#2968 = CIRCLE ( 'NONE', #5503, 2.500000000000002220 ) ;
#2969 = ORIENTED_EDGE ( 'NONE', *, *, #4831, .T. ) ;
#2970 = DIRECTION ( 'NONE',  ( -0.000000000000000000, -0.000000000000000000, -1.000000000000000000 ) ) ;
#2971 =( LENGTH_UNIT ( ) NAMED_UNIT ( * ) SI_UNIT ( .MILLI., .METRE. ) );
#2972 = DIRECTION ( 'NONE',  ( 1.000000000000000000, 0.000000000000000000, 0.000000000000000000 ) ) ;
#2973 = CARTESIAN_POINT ( 'NONE',  ( 2.000000000000001776, 0.000000000000000000, -12.44999999999999929 ) ) ;
#2974 = AXIS2_PLACEMENT_3D ( 'NONE', #10656, #4050, #6370 ) ;
#2975 = LINE ( 'NONE', #12897, #5543 ) ;
#2976 = SURFACE_SIDE_STYLE ('',( #5363 ) ) ;
#2977 = CARTESIAN_POINT ( 'NONE',  ( 4.000000000000000000, 0.3987449864460005378, -0.01220643443059817035 ) ) ;
#2978 = CONTEXT_DEPENDENT_SHAPE_REPRESENTATION ( #13175, #1710 ) ;
#2979 = ORIENTED_EDGE ( 'NONE', *, *, #13741, .T. ) ;
#2980 = DIRECTION ( 'NONE',  ( -1.000000000000000000, -0.000000000000000000, -0.000000000000000000 ) ) ;
#2981 = ORIENTED_EDGE ( 'NONE', *, *, #6675, .T. ) ;
#2982 = DIRECTION ( 'NONE',  ( 1.000000000000000000, 0.000000000000000000, 0.000000000000000000 ) ) ;
#2983 = LINE ( 'NONE', #7252, #11418 ) ;
#2984 = ORIENTED_EDGE ( 'NONE', *, *, #7793, .F. ) ;
#2985 = CARTESIAN_POINT ( 'NONE',  ( 0.000000000000000000, -2.349999999999997424, 0.5149999999999992362 ) ) ;
#2986 = ORIENTED_EDGE ( 'NONE', *, *, #10743, .F. ) ;
#2987 = CARTESIAN_POINT ( 'NONE',  ( 0.000000000000000000, -2.349999999999997424, 0.5149999999999992362 ) ) ;
#2988 = CARTESIAN_POINT ( 'NONE',  ( -4.000000000000000000, 0.000000000000000000, 0.000000000000000000 ) ) ;
#2989 = ORIENTED_EDGE ( 'NONE', *, *, #896, .F. ) ;
#2990 = DIRECTION ( 'NONE',  ( 0.000000000000000000, 0.000000000000000000, 1.000000000000000000 ) ) ;
#2991 = AXIS2_PLACEMENT_3D ( 'NONE', #11641, #7140, #4028 ) ;
#2992 = EDGE_CURVE ( 'NONE', #8157, #8189, #14213, .T. ) ;
#2993 = DIRECTION ( 'NONE',  ( 0.000000000000000000, 0.000000000000000000, -1.000000000000000000 ) ) ;
#2994 =( NAMED_UNIT ( * ) PLANE_ANGLE_UNIT ( ) SI_UNIT ( $, .RADIAN. ) );
#2995 = CARTESIAN_POINT ( 'NONE',  ( 347.0000000000000000, -8.660254037844389075, 205.0000000000000284 ) ) ;
#2996 = ITEM_DEFINED_TRANSFORMATION ( 'NONE', 'NONE', #8615,  #14039 ) ;
#2997 = CARTESIAN_POINT ( 'NONE',  ( 5.200000000000002842, 0.000000000000000000, 0.000000000000000000 ) ) ;
#2998 = VERTEX_POINT ( 'NONE', #10015 ) ;
#2999 = ORIENTED_EDGE ( 'NONE', *, *, #3883, .F. ) ;
#3000 = DIRECTION ( 'NONE',  ( 1.000000000000000000, 0.000000000000000000, 0.000000000000000000 ) ) ;
#3001 = ORIENTED_EDGE ( 'NONE', *, *, #13354, .F. ) ;
#3002 = LINE ( 'NONE', #1746, #6306 ) ;
#3003 = AXIS2_PLACEMENT_3D ( 'NONE', #9873, #1220, #5520 ) ;
#3004 = ORIENTED_EDGE ( 'NONE', *, *, #3830, .T. ) ;
#3005 = ORIENTED_EDGE ( 'NONE', *, *, #802, .T. ) ;
#3006 = FACE_BOUND ( 'NONE', #5352, .T. ) ;
#3007 = ORIENTED_EDGE ( 'NONE', *, *, #11598, .T. ) ;
#3008 = CYLINDRICAL_SURFACE ( 'NONE', #12869, 2.500000000000002220 ) ;
#3009 = UNCERTAINTY_MEASURE_WITH_UNIT (LENGTH_MEASURE( 1.000000000000000082E-05 ), #1234, 'distance_accuracy_value', 'NONE');
#3010 = DIRECTION ( 'NONE',  ( -1.000000000000000000, -0.000000000000000000, -0.000000000000000000 ) ) ;
#3011 = DIRECTION ( 'NONE',  ( 0.000000000000000000, 0.000000000000000000, 1.000000000000000000 ) ) ;
#3012 = ADVANCED_FACE ( 'NONE', ( #4434 ), #8851, .F. ) ;
#3013 = CARTESIAN_POINT ( 'NONE',  ( 140.0000000000000000, -75.00000000000008527, -190.0000000000000000 ) ) ;
#3014 = AXIS2_PLACEMENT_3D ( 'NONE', #7870, #2377, #11013 ) ;
#3015 = LINE ( 'NONE', #7210, #392 ) ;
#3016 = PRODUCT_DEFINITION_SHAPE ( 'NONE', 'NONE',  #14358 ) ;
#3017 = VERTEX_POINT ( 'NONE', #7823 ) ;
#3018 = ADVANCED_FACE ( 'NONE', ( #10894 ), #13126, .F. ) ;
#3019 = ORIENTED_EDGE ( 'NONE', *, *, #1299, .T. ) ;
#3020 = DIRECTION ( 'NONE',  ( 0.000000000000000000, 1.000000000000000000, 0.000000000000000000 ) ) ;
#3021 = CARTESIAN_POINT ( 'NONE',  ( -314.9999999999999432, -105.0000000000000995, 40.00000000000000000 ) ) ;
#3022 = CIRCLE ( 'NONE', #10422, 8.000000000000000000 ) ;
#3023 = FACE_OUTER_BOUND ( 'NONE', #12665, .T. ) ;
#3024 = FACE_BOUND ( 'NONE', #6731, .T. ) ;
#3025 = VERTEX_POINT ( 'NONE', #14140 ) ;
#3026 = AXIS2_PLACEMENT_3D ( 'NONE', #2170, #6596, #1053 ) ;
#3027 = CIRCLE ( 'NONE', #11354, 2.649999999999985700 ) ;
#3028 = FACE_BOUND ( 'NONE', #9601, .T. ) ;
#3029 = DIRECTION ( 'NONE',  ( -1.000000000000000000, 0.000000000000000000, 0.000000000000000000 ) ) ;
#3030 = DIRECTION ( 'NONE',  ( 0.000000000000000000, 0.000000000000000000, 1.000000000000000000 ) ) ;
#3031 = DIRECTION ( 'NONE',  ( -1.000000000000000000, 0.000000000000000000, 0.000000000000000000 ) ) ;
#3032 = EDGE_CURVE ( 'NONE', #9866, #7620, #9007, .T. ) ;
#3033 = PRODUCT_RELATED_PRODUCT_CATEGORY ( 'part', '', ( #7946 ) ) ;
#3034 = VERTEX_POINT ( 'NONE', #3354 ) ;
#3035 = ORIENTED_EDGE ( 'NONE', *, *, #4391, .T. ) ;
#3036 = CARTESIAN_POINT ( 'NONE',  ( -31.74999999999995737, 5.204748896376250699E-16, -4.250000000000000000 ) ) ;
#3037 = CIRCLE ( 'NONE', #13897, 0.2000000000000000944 ) ;
#3038 = CARTESIAN_POINT ( 'NONE',  ( 132.4999999999999716, 45.00000000000001421, 0.000000000000000000 ) ) ;
#3039 = PRODUCT_DEFINITION_CONTEXT ( 'detailed design', #5635, 'design' ) ;
#3040 = ORIENTED_EDGE ( 'NONE', *, *, #11028, .F. ) ;
#3041 = DIRECTION ( 'NONE',  ( 0.000000000000000000, -0.5000000000000011102, -0.8660254037844379305 ) ) ;
#3042 = ADVANCED_FACE ( 'NONE', ( #6743, #11171, #5653, #3138, #7538, #11977 ), #918, .F. ) ;
#3043 = EDGE_CURVE ( 'NONE', #6309, #12855, #994, .T. ) ;
#3044 = AXIS2_PLACEMENT_3D ( 'NONE', #8830, #12373, #20 ) ;
#3045 = CARTESIAN_POINT ( 'NONE',  ( 1.999999999999998224, -3.464101615137772594, -3.142992957459239012 ) ) ;
#3046 = CARTESIAN_POINT ( 'NONE',  ( 4.000000000000000888, -0.8578082829538523635, -3.433262215449808696 ) ) ;
#3047 = DIRECTION ( 'NONE',  ( 0.000000000000000000, 0.000000000000000000, -1.000000000000000000 ) ) ;
#3048 = CIRCLE ( 'NONE', #13450, 2.055000000000001492 ) ;
#3049 = EDGE_CURVE ( 'NONE', #11373, #8550, #8108, .T. ) ;
#3050 = ORIENTED_EDGE ( 'NONE', *, *, #5751, .T. ) ;
#3051 = CARTESIAN_POINT ( 'NONE',  ( 53.33333333333330017, -20.00000000000000000, 222.5000000000000853 ) ) ;
#3052 = AXIS2_PLACEMENT_3D ( 'NONE', #10642, #7509, #6430 ) ;
#3053 = ORIENTED_EDGE ( 'NONE', *, *, #5851, .T. ) ;
#3054 = CARTESIAN_POINT ( 'NONE',  ( 1.567478505476134803E-15, 4.618802153517012954, -3.504269196027872457 ) ) ;
#3055 = CARTESIAN_POINT ( 'NONE',  ( 299.9999999999999432, -75.00000000000008527, -190.0000000000000000 ) ) ;
#3056 =( GEOMETRIC_REPRESENTATION_CONTEXT ( 3 ) GLOBAL_UNCERTAINTY_ASSIGNED_CONTEXT ( ( #8848 ) ) GLOBAL_UNIT_ASSIGNED_CONTEXT ( ( #3641, #11616, #12775 ) ) REPRESENTATION_CONTEXT ( 'NONE', 'WORKASPACE' ) );
#3057 = ORIENTED_EDGE ( 'NONE', *, *, #11462, .F. ) ;
#3058 = DIRECTION ( 'NONE',  ( 1.000000000000000000, 0.000000000000000000, 0.000000000000000000 ) ) ;
#3059 = ORIENTED_EDGE ( 'NONE', *, *, #10660, .F. ) ;
#3060 = FACE_BOUND ( 'NONE', #1002, .T. ) ;
#3061 = EDGE_CURVE ( 'NONE', #13280, #11549, #5719, .T. ) ;
#3062 = CARTESIAN_POINT ( 'NONE',  ( -132.3499999999999943, 45.00000000000001421, 30.00000000000000000 ) ) ;
#3063 = ORIENTED_EDGE ( 'NONE', *, *, #9512, .T. ) ;
#3064 = DIRECTION ( 'NONE',  ( -1.000000000000000000, 0.000000000000000000, 0.000000000000000000 ) ) ;
#3065 = EDGE_CURVE ( 'NONE', #3461, #2019, #13474, .T. ) ;
#3066 = DIRECTION ( 'NONE',  ( 0.000000000000000000, 0.000000000000000000, 1.000000000000000000 ) ) ;
#3067 = VECTOR ( 'NONE', #5517, 1000.000000000000227 ) ;
#3068 = DIRECTION ( 'NONE',  ( 1.000000000000000000, 0.000000000000000000, 0.000000000000000000 ) ) ;
#3069 = EDGE_CURVE ( 'NONE', #5337, #9188, #2564, .T. ) ;
#3070 = ITEM_DEFINED_TRANSFORMATION ( 'NONE', 'NONE', #7909,  #14039 ) ;
#3071 = CARTESIAN_POINT ( 'NONE',  ( 5.200000000000002842, 0.000000000000000000, -2.700000000000000622 ) ) ;
#3072 = AXIS2_PLACEMENT_3D ( 'NONE', #3192, #3342, #1200 ) ;
#3073 = ORIENTED_EDGE ( 'NONE', *, *, #1797, .F. ) ;
#3074 = ORIENTED_EDGE ( 'NONE', *, *, #1737, .F. ) ;
#3075 = CARTESIAN_POINT ( 'NONE',  ( 2.500000000000000000, 3.004629197474318851E-15, 2.042000000000000259 ) ) ;
#3076 = EDGE_LOOP ( 'NONE', ( #10868, #5062, #7711, #8061 ) ) ;
#3077 = CARTESIAN_POINT ( 'NONE',  ( 2.740000000000000213, 1.042174426074397490E-16, -0.8509999999999999787 ) ) ;
#3078 = UNCERTAINTY_MEASURE_WITH_UNIT (LENGTH_MEASURE( 1.000000000000000082E-05 ), #5611, 'distance_accuracy_value', 'NONE');
#3079 = ORIENTED_EDGE ( 'NONE', *, *, #4278, .F. ) ;
#3080 = VECTOR ( 'NONE', #7090, 1000.000000000000000 ) ;
#3081 = EDGE_LOOP ( 'NONE', ( #7439, #4815, #4294 ) ) ;
#3082 = CARTESIAN_POINT ( 'NONE',  ( 305.0000000000000000, -36.99999999999997868, -169.9999999999999716 ) ) ;
#3083 = ORIENTED_EDGE ( 'NONE', *, *, #8071, .T. ) ;
#3084 = DIRECTION ( 'NONE',  ( 0.000000000000000000, 0.000000000000000000, -1.000000000000000000 ) ) ;
#3085 = AXIS2_PLACEMENT_3D ( 'NONE', #2657, #4846, #4624 ) ;
#3086 = DIRECTION ( 'NONE',  ( 0.000000000000000000, -0.4999999999999993894, 0.8660254037844389297 ) ) ;
#3087 =( GEOMETRIC_REPRESENTATION_CONTEXT ( 3 ) GLOBAL_UNCERTAINTY_ASSIGNED_CONTEXT ( ( #862 ) ) GLOBAL_UNIT_ASSIGNED_CONTEXT ( ( #515, #3884, #12372 ) ) REPRESENTATION_CONTEXT ( 'NONE', 'WORKASPACE' ) );
#3088 = DIRECTION ( 'NONE',  ( -0.000000000000000000, -0.000000000000000000, 1.000000000000000000 ) ) ;
#3089 = VECTOR ( 'NONE', #9000, 1000.000000000000000 ) ;
#3090 =( REPRESENTATION_RELATIONSHIP ('NONE','NONE', #11251, #10314 ) REPRESENTATION_RELATIONSHIP_WITH_TRANSFORMATION ( #12243 )SHAPE_REPRESENTATION_RELATIONSHIP( ) );
#3091 = CARTESIAN_POINT ( 'NONE',  ( -297.4999999999999432, -75.00000000000008527, 329.9999999999999432 ) ) ;
#3092 = CARTESIAN_POINT ( 'NONE',  ( 53.33333333333330017, -20.00000000000000000, 222.5000000000000853 ) ) ;
#3093 = AXIS2_PLACEMENT_3D ( 'NONE', #4314, #12078, #11207 ) ;
#3094 = ORIENTED_EDGE ( 'NONE', *, *, #10824, .F. ) ;
#3095 = ORIENTED_EDGE ( 'NONE', *, *, #326, .T. ) ;
#3096 = CONICAL_SURFACE ( 'NONE', #5569, 2.059999999999998721, 0.9599310885968738161 ) ;
#3097 =( GEOMETRIC_REPRESENTATION_CONTEXT ( 3 ) GLOBAL_UNCERTAINTY_ASSIGNED_CONTEXT ( ( #6293 ) ) GLOBAL_UNIT_ASSIGNED_CONTEXT ( ( #4002, #2994, #11979 ) ) REPRESENTATION_CONTEXT ( 'NONE', 'WORKASPACE' ) );
#3098 = EDGE_CURVE ( 'NONE', #5006, #9112, #13444, .T. ) ;
#3099 = CARTESIAN_POINT ( 'NONE',  ( 219.9999999999999716, -85.00000000000007105, 50.00000000000001421 ) ) ;
#3100 = ORIENTED_EDGE ( 'NONE', *, *, #5991, .T. ) ;
#3101 = FACE_OUTER_BOUND ( 'NONE', #12272, .T. ) ;
#3102 = CARTESIAN_POINT ( 'NONE',  ( 0.6937372685066666156, -4.453844082567737672, -3.610536846335894445 ) ) ;
#3103 = VECTOR ( 'NONE', #5011, 1000.000000000000000 ) ;
#3104 = DIRECTION ( 'NONE',  ( 1.000000000000000000, 0.000000000000000000, 0.000000000000000000 ) ) ;
#3105 = ORIENTED_EDGE ( 'NONE', *, *, #14237, .F. ) ;
#3106 = FACE_BOUND ( 'NONE', #12537, .T. ) ;
#3107 = DIRECTION ( 'NONE',  ( 1.000000000000000000, 0.000000000000000000, 0.000000000000000000 ) ) ;
#3108 = DIRECTION ( 'NONE',  ( 1.000000000000000000, 0.000000000000000000, 0.000000000000000000 ) ) ;
#3109 = LINE ( 'NONE', #3178, #9962 ) ;
#3110 = ORIENTED_EDGE ( 'NONE', *, *, #5180, .F. ) ;
#3111 = VERTEX_POINT ( 'NONE', #12542 ) ;
#3112 = LINE ( 'NONE', #12025, #2791 ) ;
#3113 = DIRECTION ( 'NONE',  ( 0.000000000000000000, 0.000000000000000000, -1.000000000000000000 ) ) ;
#3114 = VERTEX_POINT ( 'NONE', #252 ) ;
#3116 = EDGE_CURVE ( 'NONE', #4974, #1964, #447, .T. ) ;
#3115 = FACE_OUTER_BOUND ( 'NONE', #10481, .T. ) ;
#3117 = EDGE_CURVE ( 'NONE', #5128, #1400, #4782, .T. ) ;
#3118 = VECTOR ( 'NONE', #2319, 1000.000000000000000 ) ;
#3119 = CARTESIAN_POINT ( 'NONE',  ( -20.00000000000000000, 0.000000000000000000, 190.0000000000000000 ) ) ;
#3120 = DIRECTION ( 'NONE',  ( 1.000000000000000000, 0.000000000000000000, 0.000000000000000000 ) ) ;
#3121 = CARTESIAN_POINT ( 'NONE',  ( 0.000000000000000000, 0.000000000000000000, 0.000000000000000000 ) ) ;
#3122 = CONTEXT_DEPENDENT_SHAPE_REPRESENTATION ( #6506, #13992 ) ;
#3123 = ORIENTED_EDGE ( 'NONE', *, *, #6292, .T. ) ;
#3124 = LINE ( 'NONE', #10954, #7740 ) ;
#3125 = VERTEX_POINT ( 'NONE', #8175 ) ;
#3126 = CYLINDRICAL_SURFACE ( 'NONE', #4688, 2.500000000000000000 ) ;
#3127 = LINE ( 'NONE', #1946, #6498 ) ;
#3128 = ORIENTED_EDGE ( 'NONE', *, *, #4828, .F. ) ;
#3129 = ORIENTED_EDGE ( 'NONE', *, *, #3468, .T. ) ;
#3131 = ADVANCED_FACE ( 'NONE', ( #184 ), #12297, .F. ) ;
#3130 = DIRECTION ( 'NONE',  ( 0.000000000000000000, 0.000000000000000000, 1.000000000000000000 ) ) ;
#3132 = ADVANCED_FACE ( 'NONE', ( #3692 ), #4719, .F. ) ;
#3133 = PRODUCT_DEFINITION_SHAPE ( 'NONE', 'NONE',  #14331 ) ;
#3134 = DIRECTION ( 'NONE',  ( 0.000000000000000000, 0.000000000000000000, -1.000000000000000000 ) ) ;
#3135 = AXIS2_PLACEMENT_3D ( 'NONE', #4151, #10977, #7621 ) ;
#3136 = ORIENTED_EDGE ( 'NONE', *, *, #10935, .F. ) ;
#3137 = DIRECTION ( 'NONE',  ( 0.000000000000000000, 0.000000000000000000, 1.000000000000000000 ) ) ;
#3138 = FACE_BOUND ( 'NONE', #10695, .T. ) ;
#3139 = ADVANCED_FACE ( 'NONE', ( #13690 ), #3955, .F. ) ;
#3140 = PLANE ( 'NONE',  #9746 ) ;
#3141 = CARTESIAN_POINT ( 'NONE',  ( -299.9999999999999432, -75.00000000000008527, 0.000000000000000000 ) ) ;
#3142 = ORIENTED_EDGE ( 'NONE', *, *, #4024, .F. ) ;
#3143 = EDGE_LOOP ( 'NONE', ( #4515, #1293, #3241, #7108, #5895, #1352, #3266, #6003 ) ) ;
#3144 = ADVANCED_FACE ( 'NONE', ( #11315 ), #12605, .F. ) ;
#3145 = ADVANCED_FACE ( 'NONE', ( #7028 ), #11240, .F. ) ;
#3146 = CARTESIAN_POINT ( 'NONE',  ( 3.699999999999998401, 0.000000000000000000, 0.000000000000000000 ) ) ;
#3147 = AXIS2_PLACEMENT_3D ( 'NONE', #5594, #13624, #259 ) ;
#3148 = APPLICATION_CONTEXT ( 'automotive_design' ) ;
#3149 = CIRCLE ( 'NONE', #552, 2.649999999999985700 ) ;
#3150 = ORIENTED_EDGE ( 'NONE', *, *, #8702, .F. ) ;
#3151 = EDGE_CURVE ( 'NONE', #2165, #11325, #1493, .T. ) ;
#3152 = EDGE_CURVE ( 'NONE', #6825, #4266, #12067, .T. ) ;
#3153 = CARTESIAN_POINT ( 'NONE',  ( 259.0000000000000000, 8.660254037844390851, 199.9990000000000236 ) ) ;
#3154 = ORIENTED_EDGE ( 'NONE', *, *, #716, .F. ) ;
#3155 = ORIENTED_EDGE ( 'NONE', *, *, #13229, .F. ) ;
#3156 = DIRECTION ( 'NONE',  ( -0.000000000000000000, -0.000000000000000000, 1.000000000000000000 ) ) ;
#3157 = ORIENTED_EDGE ( 'NONE', *, *, #8229, .T. ) ;
#3158 = CARTESIAN_POINT ( 'NONE',  ( 209.9999999999999716, -85.00000000000007105, -250.0009999999999764 ) ) ;
#3159 = CARTESIAN_POINT ( 'NONE',  ( 319.9999999999999432, -25.00000000000000000, 169.9999999999999716 ) ) ;
#3160 = DIRECTION ( 'NONE',  ( 0.000000000000000000, 0.000000000000000000, 1.000000000000000000 ) ) ;
#3161 = DIRECTION ( 'NONE',  ( 0.000000000000000000, 0.000000000000000000, 1.000000000000000000 ) ) ;
#3162 = FACE_OUTER_BOUND ( 'NONE', #9051, .T. ) ;
#3163 = ORIENTED_EDGE ( 'NONE', *, *, #1155, .T. ) ;
#3164 = VERTEX_POINT ( 'NONE', #7089 ) ;
#3165 = CYLINDRICAL_SURFACE ( 'NONE', #742, 13.50000000000000355 ) ;
#3166 = CIRCLE ( 'NONE', #11714, 2.499999999999999556 ) ;
#3167 = VERTEX_POINT ( 'NONE', #10077 ) ;
#3168 = LINE ( 'NONE', #7360, #2714 ) ;
#3169 = DIRECTION ( 'NONE',  ( 0.000000000000000000, 0.000000000000000000, 1.000000000000000000 ) ) ;
#3170 = PLANE ( 'NONE',  #4834 ) ;
#3171 = EDGE_LOOP ( 'NONE', ( #8598, #4447, #2396 ) ) ;
#3172 = CIRCLE ( 'NONE', #3621, 0.8509999999999999787 ) ;
#3173 = DIRECTION ( 'NONE',  ( 1.000000000000000000, 0.000000000000000000, 0.000000000000000000 ) ) ;
#3174 = EDGE_CURVE ( 'NONE', #9742, #4689, #5798, .T. ) ;
#3175 = CIRCLE ( 'NONE', #11270, 4.000000000000000000 ) ;
#3176 = CARTESIAN_POINT ( 'NONE',  ( 3.699999999999998401, 0.000000000000000000, 0.000000000000000000 ) ) ;
#3177 = PRODUCT_CONTEXT ( 'NONE', #4616, 'mechanical' ) ;
#3178 = CARTESIAN_POINT ( 'NONE',  ( 319.9999999999999432, -225.0010000000000048, -169.9999999999999716 ) ) ;
#3179 = AXIS2_PLACEMENT_3D ( 'NONE', #8521, #6352, #10782 ) ;
#3180 = ORIENTED_EDGE ( 'NONE', *, *, #10216, .T. ) ;
#3181 = ORIENTED_EDGE ( 'NONE', *, *, #10705, .F. ) ;
#3182 = DIRECTION ( 'NONE',  ( 0.000000000000000000, 0.000000000000000000, 1.000000000000000000 ) ) ;
#3183 = VECTOR ( 'NONE', #7058, 1000.000000000000000 ) ;
#3184 = DIRECTION ( 'NONE',  ( 2.312964634635743450E-16, 1.000000000000000000, 0.000000000000000000 ) ) ;
#3185 = AXIS2_PLACEMENT_3D ( 'NONE', #9924, #1041, #4417 ) ;
#3186 = VECTOR ( 'NONE', #7303, 1000.000000000000000 ) ;
#3187 = EDGE_LOOP ( 'NONE', ( #1582, #6980, #3939, #6808 ) ) ;
#3188 = LINE ( 'NONE', #6368, #2709 ) ;
#3189 = CIRCLE ( 'NONE', #12903, 2.649999999999985700 ) ;
#3190 = CARTESIAN_POINT ( 'NONE',  ( 2.740000000000000213, -0.6774776749089230776, 0.5149999999999995692 ) ) ;
#3191 = CARTESIAN_POINT ( 'NONE',  ( 259.0000000000000000, 8.660254037844390851, 205.0000000000000284 ) ) ;
#3192 = CARTESIAN_POINT ( 'NONE',  ( 0.000000000000000000, 0.000000000000000000, 188.0000000000000000 ) ) ;
#3193 = AXIS2_PLACEMENT_3D ( 'NONE', #3715, #133, #11264 ) ;
#3194 = AXIS2_PLACEMENT_3D ( 'NONE', #10986, #10911, #14094 ) ;
#3195 = ORIENTED_EDGE ( 'NONE', *, *, #12164, .T. ) ;
#3196 = EDGE_CURVE ( 'NONE', #4280, #2907, #2391, .T. ) ;
#3197 = VECTOR ( 'NONE', #9073, 1000.000000000000000 ) ;
#3198 = CARTESIAN_POINT ( 'NONE',  ( 140.0000000000000000, -75.00000000000008527, -190.0000000000000000 ) ) ;
#3199 = AXIS2_PLACEMENT_3D ( 'NONE', #12410, #2477, #10237 ) ;
#3200 = EDGE_LOOP ( 'NONE', ( #9800, #5544 ) ) ;
#3201 = CARTESIAN_POINT ( 'NONE',  ( 16.55500000000001393, 3.061616997868383634E-16, -2.500000000000000444 ) ) ;
#3202 = DIRECTION ( 'NONE',  ( -1.000000000000000000, -0.000000000000000000, -0.000000000000000000 ) ) ;
#3203 = ORIENTED_EDGE ( 'NONE', *, *, #1169, .F. ) ;
#3204 = ORIENTED_EDGE ( 'NONE', *, *, #13931, .T. ) ;
#3205 = DIRECTION ( 'NONE',  ( 0.000000000000000000, 1.000000000000000000, 1.153406566473941260E-16 ) ) ;
#3206 = UNCERTAINTY_MEASURE_WITH_UNIT (LENGTH_MEASURE( 1.000000000000000082E-05 ), #12844, 'distance_accuracy_value', 'NONE');
#3207 = CIRCLE ( 'NONE', #12914, 2.041999999999999815 ) ;
#3208 = DIRECTION ( 'NONE',  ( 0.000000000000000000, 1.000000000000000000, 0.000000000000000000 ) ) ;
#3209 = EDGE_LOOP ( 'NONE', ( #1844, #11234, #8717, #13805 ) ) ;
#3210 = CARTESIAN_POINT ( 'NONE',  ( 347.0000000000000000, -8.660254037844389075, 200.0000000000000000 ) ) ;
#3211 = VECTOR ( 'NONE', #9099, 1000.000000000000000 ) ;
#3212 = CARTESIAN_POINT ( 'NONE',  ( 0.06760930072668813740, -0.5150000000000026779, 0.9010842325122891960 ) ) ;
#3213 = CARTESIAN_POINT ( 'NONE',  ( 0.3074992278157369086, -2.196686566159251619, -2.690165171976911629E-16 ) ) ;
#3214 = FACE_OUTER_BOUND ( 'NONE', #5311, .T. ) ;
#3215 = CONTEXT_DEPENDENT_SHAPE_REPRESENTATION ( #5093, #12369 ) ;
#3216 = CARTESIAN_POINT ( 'NONE',  ( -4.000000000000000000, 2.471528634177585282, -3.686887442155186712 ) ) ;
#3217 = VERTEX_POINT ( 'NONE', #1280 ) ;
#3218 = ORIENTED_EDGE ( 'NONE', *, *, #1527, .T. ) ;
#3219 = EDGE_CURVE ( 'NONE', #701, #11518, #13675, .T. ) ;
#3220 = FACE_OUTER_BOUND ( 'NONE', #12586, .T. ) ;
#3221 = ORIENTED_EDGE ( 'NONE', *, *, #11547, .F. ) ;
#3222 = FACE_OUTER_BOUND ( 'NONE', #8412, .T. ) ;
#3223 = ORIENTED_EDGE ( 'NONE', *, *, #11905, .F. ) ;
#3224 = VECTOR ( 'NONE', #4895, 1000.000000000000000 ) ;
#3225 = ORIENTED_EDGE ( 'NONE', *, *, #10052, .T. ) ;
#3226 = CARTESIAN_POINT ( 'NONE',  ( 0.000000000000000000, 0.000000000000000000, 190.0000000000000000 ) ) ;
#3227 = ORIENTED_EDGE ( 'NONE', *, *, #8947, .F. ) ;
#3228 = FACE_BOUND ( 'NONE', #8580, .T. ) ;
#3229 = PRODUCT ( 'angular contact ball bearing_68_iso_ISO 15 ABB - 1720 - 28,SI,NC,28_68', 'angular contact ball bearing_68_iso_ISO 15 ABB - 1720 - 28,SI,NC,28_68', '', ( #8198 ) ) ;
#3230 = FACE_OUTER_BOUND ( 'NONE', #11862, .T. ) ;
#3231 = CARTESIAN_POINT ( 'NONE',  ( 206.0000000000000284, -85.00000000000007105, 180.0000000000000000 ) ) ;
#3232 = EDGE_CURVE ( 'NONE', #8663, #10091, #917, .T. ) ;
#3233 = EDGE_CURVE ( 'NONE', #2635, #5030, #3037, .T. ) ;
#3234 = LINE ( 'NONE', #13224, #8069 ) ;
#3235 = EDGE_CURVE ( 'NONE', #10685, #7175, #9516, .T. ) ;
#3236 = CARTESIAN_POINT ( 'NONE',  ( 0.000000000000000000, 0.000000000000000000, 10.00000000000000000 ) ) ;
#3237 = VERTEX_POINT ( 'NONE', #619 ) ;
#3238 = AXIS2_PLACEMENT_3D ( 'NONE', #7957, #2460, #6956 ) ;
#3239 = ORIENTED_EDGE ( 'NONE', *, *, #1614, .F. ) ;
#3240 = CARTESIAN_POINT ( 'NONE',  ( 4.999999999999999112, -8.660254037844389075, 210.0000000000000000 ) ) ;
#3241 = ORIENTED_EDGE ( 'NONE', *, *, #3914, .T. ) ;
#3242 = DIRECTION ( 'NONE',  ( -0.000000000000000000, -0.000000000000000000, -1.000000000000000000 ) ) ;
#3243 = CARTESIAN_POINT ( 'NONE',  ( 137.4999999999999432, -56.99999999999997158, -180.0000000000000000 ) ) ;
#3244 = DIRECTION ( 'NONE',  ( -0.000000000000000000, -0.000000000000000000, 1.000000000000000000 ) ) ;
#3245 = ORIENTED_EDGE ( 'NONE', *, *, #8825, .T. ) ;
#3246 = VECTOR ( 'NONE', #13387, 1000.000000000000000 ) ;
#3247 = EDGE_CURVE ( 'NONE', #3293, #4498, #11363, .T. ) ;
#3248 = DIRECTION ( 'NONE',  ( -0.000000000000000000, -0.000000000000000000, -1.000000000000000000 ) ) ;
#3249 = LINE ( 'NONE', #13375, #9928 ) ;
#3250 = DIRECTION ( 'NONE',  ( -0.000000000000000000, -0.000000000000000000, -1.000000000000000000 ) ) ;
#3251 = ADVANCED_FACE ( 'NONE', ( #2824 ), #2894, .F. ) ;
#3252 = ORIENTED_EDGE ( 'NONE', *, *, #12759, .T. ) ;
#3253 = ORIENTED_EDGE ( 'NONE', *, *, #4457, .F. ) ;
#3254 = AXIS2_PLACEMENT_3D ( 'NONE', #12020, #6643, #4539 ) ;
#3255 = FACE_OUTER_BOUND ( 'NONE', #5659, .T. ) ;
#3256 = PRODUCT_DEFINITION_SHAPE ( 'NONE', 'NONE',  #14348 ) ;
#3257 = FACE_OUTER_BOUND ( 'NONE', #12853, .T. ) ;
#3258 = MECHANICAL_DESIGN_GEOMETRIC_PRESENTATION_REPRESENTATION (  '', ( #3737 ), #6722 ) ;
#3259 = ORIENTED_EDGE ( 'NONE', *, *, #6973, .F. ) ;
#3260 = CARTESIAN_POINT ( 'NONE',  ( 140.0000000000000000, -75.00000000000008527, 169.9999999999999716 ) ) ;
#3261 = LINE ( 'NONE', #12099, #1771 ) ;
#3262 = CARTESIAN_POINT ( 'NONE',  ( -30.00000000000002842, -20.00000000000000000, 200.0000000000000000 ) ) ;
#3263 = DIRECTION ( 'NONE',  ( 6.123233995736766036E-17, -1.000000000000000000, 0.000000000000000000 ) ) ;
#3264 = AXIS2_PLACEMENT_3D ( 'NONE', #721, #5113, #13866 ) ;
#3265 = VECTOR ( 'NONE', #13513, 999.9999999999998863 ) ;
#3266 = ORIENTED_EDGE ( 'NONE', *, *, #665, .F. ) ;
#3267 = DIRECTION ( 'NONE',  ( 0.000000000000000000, -0.4999999999999992784, 0.8660254037844389297 ) ) ;
#3268 = ORIENTED_EDGE ( 'NONE', *, *, #1868, .T. ) ;
#3269 = ADVANCED_FACE ( 'NONE', ( #1642 ), #11741, .T. ) ;
#3270 = CARTESIAN_POINT ( 'NONE',  ( 302.5000000000000000, -56.99999999999997158, -180.0000000000000000 ) ) ;
#3271 = FACE_OUTER_BOUND ( 'NONE', #6543, .T. ) ;
#3272 = AXIS2_PLACEMENT_3D ( 'NONE', #4333, #11883, #5357 ) ;
#3273 =( REPRESENTATION_RELATIONSHIP ('NONE','NONE', #11251, #2275 ) REPRESENTATION_RELATIONSHIP_WITH_TRANSFORMATION ( #12169 )SHAPE_REPRESENTATION_RELATIONSHIP( ) );
#3274 = ORIENTED_EDGE ( 'NONE', *, *, #6302, .F. ) ;
#3275 = ORIENTED_EDGE ( 'NONE', *, *, #10475, .F. ) ;
#3276 = CARTESIAN_POINT ( 'NONE',  ( 20.00000000000000000, 2.449293598294706513E-15, 190.0000000000000000 ) ) ;
#3277 = DIRECTION ( 'NONE',  ( 0.000000000000000000, 0.000000000000000000, -1.000000000000000000 ) ) ;
#3278 = DIRECTION ( 'NONE',  ( 0.4461977533473793778, -2.936240938438015166E-15, 0.8949343913984707521 ) ) ;
#3279 = CARTESIAN_POINT ( 'NONE',  ( 119.9999999999999147, -24.99999999999999289, 169.9999999999999716 ) ) ;
#3280 = CARTESIAN_POINT ( 'NONE',  ( 386.6666666666666288, -15.00000000000000000, 222.5000000000000853 ) ) ;
#3281 = CARTESIAN_POINT ( 'NONE',  ( 2.500000000000000000, -2.357898499370432166, 3.035766082959412415E-15 ) ) ;
#3282 = LINE ( 'NONE', #10019, #6027 ) ;
#3283 = ITEM_DEFINED_TRANSFORMATION ( 'NONE', 'NONE', #13481,  #14039 ) ;
#3284 = CARTESIAN_POINT ( 'NONE',  ( -2.000000000000006661, 3.464101615137750834, 0.000000000000000000 ) ) ;
#3285 = AXIS2_PLACEMENT_3D ( 'NONE', #6219, #14044, #1934 ) ;
#3286 = EDGE_LOOP ( 'NONE', ( #5040, #123, #6490, #892 ) ) ;
#3287 = ORIENTED_EDGE ( 'NONE', *, *, #6675, .F. ) ;
#3288 = CYLINDRICAL_SURFACE ( 'NONE', #13312, 9.999999999999980460 ) ;
#3289 = EDGE_LOOP ( 'NONE', ( #2068, #10541, #12566, #5550 ) ) ;
#3290 = PRESENTATION_LAYER_ASSIGNMENT (  '', '', ( #3737 ) ) ;
#3291 = DIRECTION ( 'NONE',  ( 1.000000000000000000, 7.304098846218135653E-17, -0.000000000000000000 ) ) ;
#3292 = EDGE_LOOP ( 'NONE', ( #6661, #14147 ) ) ;
#3293 = VERTEX_POINT ( 'NONE', #10659 ) ;
#3294 = LINE ( 'NONE', #5533, #13814 ) ;
#3295 = VERTEX_POINT ( 'NONE', #2973 ) ;
#3296 = DIRECTION ( 'NONE',  ( -0.000000000000000000, -0.000000000000000000, 1.000000000000000000 ) ) ;
#3297 = CYLINDRICAL_SURFACE ( 'NONE', #4577, 2.649999999999985700 ) ;
#3298 = AXIS2_PLACEMENT_3D ( 'NONE', #12642, #13800, #2718 ) ;
#3299 = CARTESIAN_POINT ( 'NONE',  ( 0.000000000000000000, -2.357898499370432610, 3.252606517456513302E-15 ) ) ;
#3300 = EDGE_CURVE ( 'NONE', #13189, #13709, #7162, .T. ) ;
#3301 = CARTESIAN_POINT ( 'NONE',  ( 2.500000000000000000, -1.178949249685214307, 2.042000000000001592 ) ) ;
#3302 = COLOUR_RGB ( '',1.000000000000000000, 0.9490196078431372140, 0.9098039215686274384 ) ;
#3303 = ADVANCED_FACE ( 'NONE', ( #465, #13761 ), #8243, .T. ) ;
#3304 = FACE_OUTER_BOUND ( 'NONE', #501, .T. ) ;
#3305 = FACE_OUTER_BOUND ( 'NONE', #3839, .T. ) ;
#3306 = VERTEX_POINT ( 'NONE', #1716 ) ;
#3307 = ORIENTED_EDGE ( 'NONE', *, *, #5685, .T. ) ;
#3308 = AXIS2_PLACEMENT_3D ( 'NONE', #6678, #5586, #7887 ) ;
#3309 = EDGE_CURVE ( 'NONE', #5369, #2602, #11593, .T. ) ;
#3310 = DIRECTION ( 'NONE',  ( 0.000000000000000000, 1.000000000000000000, 0.000000000000000000 ) ) ;
#3311 = AXIS2_PLACEMENT_3D ( 'NONE', #4271, #9999, #30 ) ;
#3312 = VERTEX_POINT ( 'NONE', #6081 ) ;
#3313 = DIRECTION ( 'NONE',  ( 0.000000000000000000, 0.000000000000000000, 1.000000000000000000 ) ) ;
#3314 = VECTOR ( 'NONE', #12269, 1000.000000000000000 ) ;
#3315 = DIRECTION ( 'NONE',  ( -1.000000000000000000, -0.000000000000000000, -0.000000000000000000 ) ) ;
#3316 = CARTESIAN_POINT ( 'NONE',  ( 469.9999999999998863, -225.0000000000000000, 169.9999999999999716 ) ) ;
#3317 = VERTEX_POINT ( 'NONE', #6296 ) ;
#3318 = EDGE_CURVE ( 'NONE', #13543, #6044, #7383, .T. ) ;
#3319 = VECTOR ( 'NONE', #9421, 1000.000000000000000 ) ;
#3320 = FACE_OUTER_BOUND ( 'NONE', #3286, .T. ) ;
#3321 = CARTESIAN_POINT ( 'NONE',  ( -304.9999999999999432, 45.00000000000001421, 30.00000000000000000 ) ) ;
#3322 = PRODUCT_DEFINITION_FORMATION_WITH_SPECIFIED_SOURCE ( 'ANY', '', #3346, .NOT_KNOWN. ) ;
#3323 = CARTESIAN_POINT ( 'NONE',  ( 219.9999999999999716, -20.00000000000000000, 225.1500000000000625 ) ) ;
#3324 = DIRECTION ( 'NONE',  ( 0.000000000000000000, -2.105246936865057050E-16, -1.000000000000000000 ) ) ;
#3325 = EDGE_CURVE ( 'NONE', #2471, #14086, #2126, .T. ) ;
#3326 = VECTOR ( 'NONE', #6308, 1000.000000000000000 ) ;
#3327 = ORIENTED_EDGE ( 'NONE', *, *, #9058, .F. ) ;
#3328 = ADVANCED_FACE ( 'NONE', ( #11814 ), #12731, .F. ) ;
#3329 = EDGE_CURVE ( 'NONE', #5679, #2529, #2361, .T. ) ;
#3330 = CARTESIAN_POINT ( 'NONE',  ( 2.500000000000000000, 1.768423874527824902, 1.020999999999999019 ) ) ;
#3331 = CIRCLE ( 'NONE', #8165, 5.000000000000004441 ) ;
#3332 = ADVANCED_FACE ( 'NONE', ( #151 ), #1384, .T. ) ;
#3333 = EDGE_CURVE ( 'NONE', #3475, #4527, #1185, .T. ) ;
#3334 = DIRECTION ( 'NONE',  ( 0.000000000000000000, 0.000000000000000000, -1.000000000000000000 ) ) ;
#3335 = ORIENTED_EDGE ( 'NONE', *, *, #3232, .F. ) ;
#3336 = CARTESIAN_POINT ( 'NONE',  ( 140.0000000000000000, -75.00000000000008527, 186.2999999999999829 ) ) ;
#3337 = ORIENTED_EDGE ( 'NONE', *, *, #14276, .F. ) ;
#3338 = CARTESIAN_POINT ( 'NONE',  ( 140.0000000000000000, -75.00000000000008527, -190.0000000000000000 ) ) ;
#3339 = EDGE_CURVE ( 'NONE', #2239, #5230, #5127, .T. ) ;
#3340 = LINE ( 'NONE', #13319, #6672 ) ;
#3341 = LINE ( 'NONE', #93, #1357 ) ;
#3342 = DIRECTION ( 'NONE',  ( 1.000000000000000000, 0.000000000000000000, 0.000000000000000000 ) ) ;
#3343 = AXIS2_PLACEMENT_3D ( 'NONE', #12052, #13062, #13273 ) ;
#3344 = VERTEX_POINT ( 'NONE', #10114 ) ;
#3345 = DIRECTION ( 'NONE',  ( -1.000000000000000000, -0.000000000000000000, -0.000000000000000000 ) ) ;
#3346 = PRODUCT ( 'socket head cap screw_iso_ISO 4762 M5 x 16 - 16N', 'socket head cap screw_iso_ISO 4762 M5 x 16 - 16N', '', ( #4668 ) ) ;
#3347 = EDGE_LOOP ( 'NONE', ( #4482, #14162 ) ) ;
#3348 = CARTESIAN_POINT ( 'NONE',  ( -4.000000000000000000, 0.000000000000000000, 0.000000000000000000 ) ) ;
#3349 = VERTEX_POINT ( 'NONE', #9984 ) ;
#3350 = ORIENTED_EDGE ( 'NONE', *, *, #3883, .T. ) ;
#3351 = CARTESIAN_POINT ( 'NONE',  ( -1.999999999999998224, 0.000000000000000000, -11.05000000000000071 ) ) ;
#3352 = FACE_OUTER_BOUND ( 'NONE', #7813, .T. ) ;
#3353 = DIRECTION ( 'NONE',  ( 1.000000000000000000, 0.000000000000000000, 0.000000000000000000 ) ) ;
#3354 = CARTESIAN_POINT ( 'NONE',  ( 238.9999999999999432, -85.00000000000007105, 190.0000000000000000 ) ) ;
#3355 = DIRECTION ( 'NONE',  ( -0.000000000000000000, 1.000000000000000000, -0.000000000000000000 ) ) ;
#3356 = FACE_OUTER_BOUND ( 'NONE', #6908, .T. ) ;
#3357 = ADVANCED_FACE ( 'NONE', ( #77 ), #5296, .F. ) ;
#3358 = LINE ( 'NONE', #6606, #2295 ) ;
#3359 = ITEM_DEFINED_TRANSFORMATION ( 'NONE', 'NONE', #7223,  #14039 ) ;
#3360 = CARTESIAN_POINT ( 'NONE',  ( -0.6507732100473471171, 4.243078065514775510, -0.2236248678334823436 ) ) ;
#3361 = EDGE_LOOP ( 'NONE', ( #5617, #8935, #2202, #9522 ) ) ;
#3362 = EDGE_LOOP ( 'NONE', ( #3792, #12684, #11851, #10750 ) ) ;
#3363 = DIRECTION ( 'NONE',  ( -1.000000000000000000, 0.000000000000000000, 0.000000000000000000 ) ) ;
#3364 = ORIENTED_EDGE ( 'NONE', *, *, #1687, .F. ) ;
#3365 = CARTESIAN_POINT ( 'NONE',  ( 297.3499999999999659, -75.00000000000008527, 169.9999999999999716 ) ) ;
#3366 = VERTEX_POINT ( 'NONE', #7858 ) ;
#3367 = FACE_OUTER_BOUND ( 'NONE', #7390, .T. ) ;
#3368 = ORIENTED_EDGE ( 'NONE', *, *, #13609, .T. ) ;
#3369 = DIRECTION ( 'NONE',  ( -0.000000000000000000, 0.000000000000000000, -1.000000000000000000 ) ) ;
#3370 = FACE_OUTER_BOUND ( 'NONE', #12461, .T. ) ;
#3371 = CARTESIAN_POINT ( 'NONE',  ( 0.2500000000000002220, 0.000000000000000000, 0.000000000000000000 ) ) ;
#3372 = ADVANCED_FACE ( 'NONE', ( #13373 ), #13445, .T. ) ;
#3373 = DIRECTION ( 'NONE',  ( 1.000000000000000000, 0.000000000000000000, 0.000000000000000000 ) ) ;
#3374 = VECTOR ( 'NONE', #6254, 1000.000000000000000 ) ;
#3375 = EDGE_LOOP ( 'NONE', ( #9305, #6235 ) ) ;
#3376 = CONICAL_SURFACE ( 'NONE', #13535, 2.041999999999999815, 1.047197551196591858 ) ;
#3377 = VERTEX_POINT ( 'NONE', #4405 ) ;
#3378 = ADVANCED_FACE ( 'NONE', ( #4476 ), #1106, .F. ) ;
#3379 = CARTESIAN_POINT ( 'NONE',  ( 3.900000000000000799, 3.306546357697853733E-16, -2.700000000000000178 ) ) ;
#3380 = VERTEX_POINT ( 'NONE', #12367 ) ;
#3381 = DIRECTION ( 'NONE',  ( 0.000000000000000000, 0.000000000000000000, -1.000000000000000000 ) ) ;
#3382 = CARTESIAN_POINT ( 'NONE',  ( 2.500000000000000000, 2.357898499370431722, -2.818925648462311528E-15 ) ) ;
#3383 = DIRECTION ( 'NONE',  ( 1.000000000000000000, 0.000000000000000000, 0.000000000000000000 ) ) ;
#3384 = EDGE_LOOP ( 'NONE', ( #10536, #12548 ) ) ;
#3385 = SHAPE_REPRESENTATION ( 'actuator', ( #14039 ), #1410 ) ;
#3386 = DIRECTION ( 'NONE',  ( 0.000000000000000000, 0.000000000000000000, 1.000000000000000000 ) ) ;
#3387 = CARTESIAN_POINT ( 'NONE',  ( -30.00000000000002842, 15.00000000000000000, 205.0000000000000284 ) ) ;
#3388 = DIRECTION ( 'NONE',  ( 0.000000000000000000, 0.000000000000000000, 1.000000000000000000 ) ) ;
#3389 = CARTESIAN_POINT ( 'NONE',  ( -4.154094228333820915, -2.398367420967594921, -3.721909803043257803 ) ) ;
#3390 = ORIENTED_EDGE ( 'NONE', *, *, #11119, .F. ) ;
#3391 = CIRCLE ( 'NONE', #11486, 2.649999999999985700 ) ;
#3392 = AXIS2_PLACEMENT_3D ( 'NONE', #13263, #5708, #7742 ) ;
#3393 = ADVANCED_FACE ( 'NONE', ( #8955 ), #2090, .F. ) ;
#3394 = DIRECTION ( 'NONE',  ( -0.000000000000000000, -1.000000000000000000, -0.000000000000000000 ) ) ;
#3395 = PLANE ( 'NONE',  #8036 ) ;
#3396 = ORIENTED_EDGE ( 'NONE', *, *, #13670, .F. ) ;
#3397 = CARTESIAN_POINT ( 'NONE',  ( 0.000000000000000000, -2.357898499370432166, 3.035766082959412415E-15 ) ) ;
#3398 = CARTESIAN_POINT ( 'NONE',  ( 0.2500000000000002220, 0.000000000000000000, 0.000000000000000000 ) ) ;
#3399 = EDGE_CURVE ( 'NONE', #13571, #11552, #12, .T. ) ;
#3400 = EDGE_CURVE ( 'NONE', #11973, #11685, #13232, .T. ) ;
#3401 = CIRCLE ( 'NONE', #12227, 11.05000000000000071 ) ;
#3402 = CARTESIAN_POINT ( 'NONE',  ( 140.0000000000000000, -95.00000000000008527, -186.2999999999999829 ) ) ;
#3403 = DIRECTION ( 'NONE',  ( 0.000000000000000000, 0.000000000000000000, 1.000000000000000000 ) ) ;
#3404 = EDGE_CURVE ( 'NONE', #6208, #10596, #8894, .T. ) ;
#3405 = CIRCLE ( 'NONE', #9410, 2.649999999999985700 ) ;
#3406 = VERTEX_POINT ( 'NONE', #3387 ) ;
#3407 = VECTOR ( 'NONE', #617, 1000.000000000000000 ) ;
#3408 = CARTESIAN_POINT ( 'NONE',  ( 79.99999999999971578, 35.00000000000000000, 0.000000000000000000 ) ) ;
#3409 = VECTOR ( 'NONE', #6262, 1000.000000000000114 ) ;
#3410 = ORIENTED_EDGE ( 'NONE', *, *, #12867, .F. ) ;
#3411 = DIRECTION ( 'NONE',  ( 1.000000000000000000, 0.000000000000000000, 0.000000000000000000 ) ) ;
#3412 = AXIS2_PLACEMENT_3D ( 'NONE', #4033, #11717, #5338 ) ;
#3413 = ORIENTED_EDGE ( 'NONE', *, *, #6989, .T. ) ;
#3414 = ORIENTED_EDGE ( 'NONE', *, *, #6848, .T. ) ;
#3415 = DIRECTION ( 'NONE',  ( 0.000000000000000000, -0.000000000000000000, -1.000000000000000000 ) ) ;
#3416 = CARTESIAN_POINT ( 'NONE',  ( 307.4999999999999432, 45.00000000000001421, 0.000000000000000000 ) ) ;
#3417 = VECTOR ( 'NONE', #9163, 1000.000000000000000 ) ;
#3418 = APPLICATION_CONTEXT ( 'automotive_design' ) ;
#3419 = DIRECTION ( 'NONE',  ( 1.000000000000000000, 0.000000000000000000, 0.000000000000000000 ) ) ;
#3420 = CARTESIAN_POINT ( 'NONE',  ( -20.63749999999999574, 1.653273178848927261E-15, 13.50000000000000355 ) ) ;
#3421 = LINE ( 'NONE', #10078, #12546 ) ;
#3422 = PLANE ( 'NONE',  #7552 ) ;
#3423 =( NAMED_UNIT ( * ) PLANE_ANGLE_UNIT ( ) SI_UNIT ( $, .RADIAN. ) );
#3424 = CARTESIAN_POINT ( 'NONE',  ( 0.000000000000000000, 0.000000000000000000, -200.0000000000000000 ) ) ;
#3425 = FACE_OUTER_BOUND ( 'NONE', #10799, .T. ) ;
#3426 = VECTOR ( 'NONE', #5119, 1000.000000000000000 ) ;
#3427 = EDGE_LOOP ( 'NONE', ( #13700, #9566, #11098, #4797 ) ) ;
#3428 = ORIENTED_EDGE ( 'NONE', *, *, #7357, .F. ) ;
#3429 = DIRECTION ( 'NONE',  ( -0.000000000000000000, 1.000000000000000000, -0.000000000000000000 ) ) ;
#3430 = CIRCLE ( 'NONE', #2962, 13.29999999999999893 ) ;
#3431 = ORIENTED_EDGE ( 'NONE', *, *, #720, .T. ) ;
#3432 = DIRECTION ( 'NONE',  ( -1.000000000000000000, 0.000000000000000000, 0.000000000000000000 ) ) ;
#3433 = COLOUR_RGB ( '',0.8941176470588234615, 0.8941176470588234615, 0.8941176470588234615 ) ;
#3434 = EDGE_CURVE ( 'NONE', #5319, #11916, #223, .T. ) ;
#3435 = ORIENTED_EDGE ( 'NONE', *, *, #12521, .T. ) ;
#3436 = DIRECTION ( 'NONE',  ( 1.000000000000000000, 0.000000000000000000, 0.000000000000000000 ) ) ;
#3437 = EDGE_LOOP ( 'NONE', ( #13630, #12058 ) ) ;
#3438 = DIRECTION ( 'NONE',  ( -1.000000000000000000, -0.000000000000000000, -0.000000000000000000 ) ) ;
#3439 = DIRECTION ( 'NONE',  ( -0.000000000000000000, -0.000000000000000000, 1.000000000000000000 ) ) ;
#3440 = DIRECTION ( 'NONE',  ( 1.000000000000000000, 0.000000000000000000, 0.000000000000000000 ) ) ;
#3441 = DIRECTION ( 'NONE',  ( 0.8949343913984143528, 0.4461977533474922875, 0.000000000000000000 ) ) ;
#3442 = DIRECTION ( 'NONE',  ( 1.000000000000000000, 0.000000000000000000, 6.123233995736766036E-17 ) ) ;
#3443 = CIRCLE ( 'NONE', #1094, 0.4499999999999985678 ) ;
#3444 = LINE ( 'NONE', #1380, #9685 ) ;
#3445 = ORIENTED_EDGE ( 'NONE', *, *, #1764, .F. ) ;
#3446 = VECTOR ( 'NONE', #2715, 1000.000000000000000 ) ;
#3447 = ORIENTED_EDGE ( 'NONE', *, *, #10294, .F. ) ;
#3448 = DIRECTION ( 'NONE',  ( 1.000000000000000000, 0.000000000000000000, -0.000000000000000000 ) ) ;
#3449 = EDGE_CURVE ( 'NONE', #6255, #1188, #7786, .T. ) ;
#3450 = ORIENTED_EDGE ( 'NONE', *, *, #13548, .T. ) ;
#3451 = CARTESIAN_POINT ( 'NONE',  ( 119.9999999999999147, -20.00000000000000000, 19.99999999999998934 ) ) ;
#3452 = DIRECTION ( 'NONE',  ( 0.000000000000000000, 0.000000000000000000, 1.000000000000000000 ) ) ;
#3453 = SURFACE_SIDE_STYLE ('',( #12218 ) ) ;
#3454 = LINE ( 'NONE', #5627, #12535 ) ;
#3455 = CARTESIAN_POINT ( 'NONE',  ( 4.000000000000000000, 2.512223110932545023, -3.469391141908803711 ) ) ;
#3456 = EDGE_CURVE ( 'NONE', #2766, #7253, #4433, .T. ) ;
#3457 = CIRCLE ( 'NONE', #6920, 5.000000000000004441 ) ;
#3458 = CARTESIAN_POINT ( 'NONE',  ( 242.4999999999999716, -80.00000000000007105, 55.00000000000001421 ) ) ;
#3459 = PRODUCT ( 'axis', 'axis', '', ( #5025 ) ) ;
#3460 = DIRECTION ( 'NONE',  ( 1.000000000000000000, 0.000000000000000000, 0.000000000000000000 ) ) ;
#3461 = VERTEX_POINT ( 'NONE', #8073 ) ;
#3462 = CYLINDRICAL_SURFACE ( 'NONE', #12998, 2.649999999999985700 ) ;
#3463 = VECTOR ( 'NONE', #10584, 999.9999999999998863 ) ;
#3464 = DIRECTION ( 'NONE',  ( 0.000000000000000000, 1.000000000000000000, 0.000000000000000000 ) ) ;
#3465 = PLANE ( 'NONE',  #142 ) ;
#3466 = EDGE_LOOP ( 'NONE', ( #2062, #7298, #14098, #9821, #343, #13771, #1562, #1180 ) ) ;
#3467 = CARTESIAN_POINT ( 'NONE',  ( -1.799999999999996048, 0.000000000000000000, 0.000000000000000000 ) ) ;
#3468 = EDGE_CURVE ( 'NONE', #5358, #6474, #11848, .T. ) ;
#3469 = CARTESIAN_POINT ( 'NONE',  ( 294.4999999999999432, -75.00000000000008527, -186.2999999999999829 ) ) ;
#3470 = DIRECTION ( 'NONE',  ( 0.000000000000000000, 0.000000000000000000, 1.000000000000000000 ) ) ;
#3471 = ADVANCED_FACE ( 'NONE', ( #10550 ), #2813, .F. ) ;
#3472 = AXIS2_PLACEMENT_3D ( 'NONE', #9114, #5849, #8381 ) ;
#3473 = ORIENTED_EDGE ( 'NONE', *, *, #947, .F. ) ;
#3474 = DIRECTION ( 'NONE',  ( 0.000000000000000000, -0.5000000000000011102, -0.8660254037844379305 ) ) ;
#3475 = VERTEX_POINT ( 'NONE', #433 ) ;
#3476 = CARTESIAN_POINT ( 'NONE',  ( 1.243802165048773611, -3.900692638707475624, -3.223146290109810241 ) ) ;
#3477 = EDGE_CURVE ( 'NONE', #4689, #9742, #10450, .T. ) ;
#3478 = VERTEX_POINT ( 'NONE', #12722 ) ;
#3479 = EDGE_LOOP ( 'NONE', ( #3545, #1296, #9689, #9133 ) ) ;
#3480 = DIRECTION ( 'NONE',  ( -0.000000000000000000, 1.000000000000000000, 1.224646799147353207E-16 ) ) ;
#3481 = CARTESIAN_POINT ( 'NONE',  ( 1.390230914382191596, 4.043987460488659202, -3.502507215260488582 ) ) ;
#3482 = VECTOR ( 'NONE', #1783, 1000.000000000000000 ) ;
#3483 = DIRECTION ( 'NONE',  ( 1.000000000000000000, 0.000000000000000000, 0.000000000000000000 ) ) ;
#3484 = VECTOR ( 'NONE', #750, 1000.000000000000000 ) ;
#3485 = EDGE_CURVE ( 'NONE', #10176, #13937, #2645, .T. ) ;
#3486 = DIRECTION ( 'NONE',  ( -0.000000000000000000, -0.000000000000000000, -1.000000000000000000 ) ) ;
#3487 = FACE_OUTER_BOUND ( 'NONE', #8187, .T. ) ;
#3488 = DIRECTION ( 'NONE',  ( 0.000000000000000000, 0.000000000000000000, -1.000000000000000000 ) ) ;
#3489 = CIRCLE ( 'NONE', #4155, 4.556291390728477886 ) ;
#3490 = LINE ( 'NONE', #8709, #8304 ) ;
#3491 = VERTEX_POINT ( 'NONE', #9320 ) ;
#3492 = ORIENTED_EDGE ( 'NONE', *, *, #12141, .T. ) ;
#3493 = DIRECTION ( 'NONE',  ( -0.000000000000000000, -0.000000000000000000, 1.000000000000000000 ) ) ;
#3494 = AXIS2_PLACEMENT_3D ( 'NONE', #9933, #1128, #7019 ) ;
#3495 = ORIENTED_EDGE ( 'NONE', *, *, #3576, .T. ) ;
#3496 = AXIS2_PLACEMENT_3D ( 'NONE', #10250, #12495, #12634 ) ;
#3497 = CARTESIAN_POINT ( 'NONE',  ( 93.00000000000000000, 8.660254037844390851, 200.0000000000000000 ) ) ;
#3498 = EDGE_CURVE ( 'NONE', #5927, #9740, #8599, .T. ) ;
#3499 = ORIENTED_EDGE ( 'NONE', *, *, #4750, .F. ) ;
#3500 = ADVANCED_FACE ( 'NONE', ( #11563 ), #5905, .F. ) ;
#3501 = CARTESIAN_POINT ( 'NONE',  ( 299.9999999999999432, -95.00000000000008527, -186.2999999999999829 ) ) ;
#3502 = ORIENTED_EDGE ( 'NONE', *, *, #13999, .F. ) ;
#3503 = VECTOR ( 'NONE', #6008, 1000.000000000000000 ) ;
#3504 = DIRECTION ( 'NONE',  ( 0.000000000000000000, 0.000000000000000000, 1.000000000000000000 ) ) ;
#3505 = DIRECTION ( 'NONE',  ( 0.000000000000000000, 0.000000000000000000, 1.000000000000000000 ) ) ;
#3506 = DIRECTION ( 'NONE',  ( 1.000000000000000000, 0.000000000000000000, 0.000000000000000000 ) ) ;
#3507 = EDGE_CURVE ( 'NONE', #1452, #1662, #4970, .T. ) ;
#3508 = FACE_OUTER_BOUND ( 'NONE', #2046, .T. ) ;
#3509 = FILL_AREA_STYLE_COLOUR ( '', #4701 ) ;
#3510 = VECTOR ( 'NONE', #12822, 1000.000000000000000 ) ;
#3511 = CARTESIAN_POINT ( 'NONE',  ( -2.500000000000000444, 3.061616997868383634E-16, -25.03750572909317285 ) ) ;
#3512 = CARTESIAN_POINT ( 'NONE',  ( 0.000000000000000000, 0.000000000000000000, 186.0000000000000000 ) ) ;
#3513 = ORIENTED_EDGE ( 'NONE', *, *, #12353, .F. ) ;
#3514 = EDGE_LOOP ( 'NONE', ( #13682, #11484, #3274 ) ) ;
#3515 = ORIENTED_EDGE ( 'NONE', *, *, #3988, .F. ) ;
#3516 = FACE_OUTER_BOUND ( 'NONE', #6090, .T. ) ;
#3517 = VECTOR ( 'NONE', #299, 1000.000000000000000 ) ;
#3518 = ORIENTED_EDGE ( 'NONE', *, *, #4544, .F. ) ;
#3519 = DIRECTION ( 'NONE',  ( -1.000000000000000000, 0.000000000000000000, 0.000000000000000000 ) ) ;
#3520 = DIRECTION ( 'NONE',  ( 1.000000000000000000, 0.000000000000000000, 0.000000000000000000 ) ) ;
#3521 = DIRECTION ( 'NONE',  ( -0.000000000000000000, 1.000000000000000000, -0.000000000000000000 ) ) ;
#3522 = DIRECTION ( 'NONE',  ( 0.000000000000000000, 0.000000000000000000, 1.000000000000000000 ) ) ;
#3523 = DIRECTION ( 'NONE',  ( -1.000000000000000000, 0.000000000000000000, 0.000000000000000000 ) ) ;
#3524 = CARTESIAN_POINT ( 'NONE',  ( -307.6499999999999204, 45.00000000000001421, 30.00000000000000000 ) ) ;
#3525 = AXIS2_PLACEMENT_3D ( 'NONE', #10151, #1216, #9060 ) ;
#3526 = FACE_OUTER_BOUND ( 'NONE', #12309, .T. ) ;
#3527 = EDGE_CURVE ( 'NONE', #6597, #6422, #9989, .T. ) ;
#3528 = CONICAL_SURFACE ( 'NONE', #5353, 2.041999999999999815, 1.047197551196591858 ) ;
#3529 = ORIENTED_EDGE ( 'NONE', *, *, #13666, .F. ) ;
#3530 = AXIS2_PLACEMENT_3D ( 'NONE', #4552, #1267, #5704 ) ;
#3531 = CARTESIAN_POINT ( 'NONE',  ( 4.999999999999999112, 0.000000000000000000, -200.0000000000000000 ) ) ;
#3532 = DIRECTION ( 'NONE',  ( 0.000000000000000000, 0.000000000000000000, 1.000000000000000000 ) ) ;
#3533 = FACE_BOUND ( 'NONE', #9400, .T. ) ;
#3534 = ORIENTED_EDGE ( 'NONE', *, *, #8685, .T. ) ;
#3535 = AXIS2_PLACEMENT_3D ( 'NONE', #6279, #3966, #600 ) ;
#3536 = DIRECTION ( 'NONE',  ( -0.000000000000000000, -0.000000000000000000, -1.000000000000000000 ) ) ;
#3537 = LINE ( 'NONE', #7941, #3923 ) ;
#3538 = CARTESIAN_POINT ( 'NONE',  ( 219.9999999999999716, -30.00000000000000355, -222.5000000000000853 ) ) ;
#3539 = ADVANCED_FACE ( 'NONE', ( #11426 ), #6123, .T. ) ;
#3540 =( REPRESENTATION_RELATIONSHIP ('NONE','NONE', #11251, #10713 ) REPRESENTATION_RELATIONSHIP_WITH_TRANSFORMATION ( #12610 )SHAPE_REPRESENTATION_RELATIONSHIP( ) );
#3541 = CIRCLE ( 'NONE', #2855, 0.2000000000000022593 ) ;
#3542 = ORIENTED_EDGE ( 'NONE', *, *, #11289, .F. ) ;
#3543 = DIRECTION ( 'NONE',  ( 0.000000000000000000, 0.000000000000000000, 1.000000000000000000 ) ) ;
#3544 = FACE_BOUND ( 'NONE', #1673, .T. ) ;
#3545 = ORIENTED_EDGE ( 'NONE', *, *, #5646, .T. ) ;
#3546 = DIRECTION ( 'NONE',  ( -1.000000000000000000, -0.000000000000000000, -0.000000000000000000 ) ) ;
#3547 = ADVANCED_FACE ( 'NONE', ( #10261 ), #3730, .F. ) ;
#3548 = EDGE_CURVE ( 'NONE', #1708, #10304, #2575, .T. ) ;
#3549 = ORIENTED_EDGE ( 'NONE', *, *, #9332, .F. ) ;
#3550 = ORIENTED_EDGE ( 'NONE', *, *, #13548, .F. ) ;
#3551 = FACE_BOUND ( 'NONE', #11332, .T. ) ;
#3552 = CARTESIAN_POINT ( 'NONE',  ( 4.175002511812151873, 2.208363329454889445, -3.469254087858244073 ) ) ;
#3553 = CARTESIAN_POINT ( 'NONE',  ( 444.9999999999999432, 8.660254037844390851, 199.9990000000000236 ) ) ;
#3554 = CARTESIAN_POINT ( 'NONE',  ( 0.000000000000000000, 1.438959988998140160E-15, -11.75000000000000000 ) ) ;
#3555 = DIRECTION ( 'NONE',  ( -1.000000000000000000, 0.000000000000000000, 0.000000000000000000 ) ) ;
#3556 = FACE_OUTER_BOUND ( 'NONE', #8722, .T. ) ;
#3557 = DIRECTION ( 'NONE',  ( 0.000000000000000000, -0.5000000000000012212, -0.8660254037844380415 ) ) ;
#3558 = ORIENTED_EDGE ( 'NONE', *, *, #1827, .F. ) ;
#3559 = ORIENTED_EDGE ( 'NONE', *, *, #940, .F. ) ;
#3560 = CARTESIAN_POINT ( 'NONE',  ( -124.9999999999999432, -105.0000000000000853, 40.00000000000000000 ) ) ;
#3561 = ORIENTED_EDGE ( 'NONE', *, *, #8052, .T. ) ;
#3562 = CARTESIAN_POINT ( 'NONE',  ( 119.9999999999999147, -225.0010000000000048, -19.99999999999998934 ) ) ;
#3563 = EDGE_CURVE ( 'NONE', #2924, #11304, #5047, .T. ) ;
#3564 = EDGE_CURVE ( 'NONE', #9136, #8882, #2506, .T. ) ;
#3565 = ORIENTED_EDGE ( 'NONE', *, *, #1868, .F. ) ;
#3566 = FACE_BOUND ( 'NONE', #13187, .T. ) ;
#3567 = ORIENTED_EDGE ( 'NONE', *, *, #3548, .T. ) ;
#3568 = DIRECTION ( 'NONE',  ( 1.000000000000000000, 0.000000000000000000, 0.000000000000000000 ) ) ;
#3569 = PRODUCT_DEFINITION_SHAPE ( 'NONE', 'NONE',  #14322 ) ;
#3570 = DIRECTION ( 'NONE',  ( 0.000000000000000000, 0.000000000000000000, -1.000000000000000000 ) ) ;
#3571 = DIRECTION ( 'NONE',  ( 1.000000000000000000, 0.000000000000000000, 0.000000000000000000 ) ) ;
#3572 = CYLINDRICAL_SURFACE ( 'NONE', #9498, 2.649999999999985700 ) ;
#3573 =( NAMED_UNIT ( * ) SI_UNIT ( $, .STERADIAN. ) SOLID_ANGLE_UNIT ( ) );
#3574 = MANIFOLD_SOLID_BREP ( 'AdvancedHole2', #4054 ) ;
#3575 = FACE_OUTER_BOUND ( 'NONE', #14225, .T. ) ;
#3576 = EDGE_CURVE ( 'NONE', #7514, #2464, #7350, .T. ) ;
#3577 = EDGE_CURVE ( 'NONE', #12823, #5253, #455, .T. ) ;
#3578 = CARTESIAN_POINT ( 'NONE',  ( 2.740000000000000213, 0.000000000000000000, 0.000000000000000000 ) ) ;
#3579 = ORIENTED_EDGE ( 'NONE', *, *, #3749, .F. ) ;
#3580 = EDGE_CURVE ( 'NONE', #8981, #1904, #7440, .T. ) ;
#3581 = VERTEX_POINT ( 'NONE', #1979 ) ;
#3582 = VERTEX_POINT ( 'NONE', #9686 ) ;
#3583 = PLANE ( 'NONE',  #6507 ) ;
#3584 = VERTEX_POINT ( 'NONE', #7278 ) ;
#3585 = DIRECTION ( 'NONE',  ( -1.000000000000000000, -0.000000000000000000, -0.000000000000000000 ) ) ;
#3586 = ORIENTED_EDGE ( 'NONE', *, *, #8634, .F. ) ;
#3587 = DIRECTION ( 'NONE',  ( -1.000000000000000000, -0.000000000000000000, -0.000000000000000000 ) ) ;
#3588 = DIRECTION ( 'NONE',  ( 0.000000000000000000, 0.000000000000000000, 1.000000000000000000 ) ) ;
#3589 = CLOSED_SHELL ( 'NONE', ( #3131, #10392, #8160, #2686, #1791, #919, #12214, #8081, #4643, #12876, #7286, #10456, #5274, #5350, #362, #12962, #6089, #5007, #11103, #1251, #9468, #9610, #10646, #10107, #4962, #3751, #2164, #9040, #141, #12685, #3139, #529, #472, #11366 ) ) ;
#3590 = CARTESIAN_POINT ( 'NONE',  ( 2.500000000000000000, 0.000000000000000000, 0.000000000000000000 ) ) ;
#3591 = CARTESIAN_POINT ( 'NONE',  ( 134.9999999999999432, -56.99999999999997158, 10.00000000000000178 ) ) ;
#3592 = FACE_OUTER_BOUND ( 'NONE', #11896, .T. ) ;
#3593 = DIRECTION ( 'NONE',  ( 0.000000000000000000, 0.000000000000000000, 1.000000000000000000 ) ) ;
#3594 = VERTEX_POINT ( 'NONE', #12801 ) ;
#3595 =( REPRESENTATION_RELATIONSHIP ('NONE','NONE', #11251, #208 ) REPRESENTATION_RELATIONSHIP_WITH_TRANSFORMATION ( #2996 )SHAPE_REPRESENTATION_RELATIONSHIP( ) );
#3596 = AXIS2_PLACEMENT_3D ( 'NONE', #13092, #6434, #8824 ) ;
#3597 = DIRECTION ( 'NONE',  ( -1.000000000000000000, 0.000000000000000000, 0.000000000000000000 ) ) ;
#3598 = CARTESIAN_POINT ( 'NONE',  ( -2.000000000000006661, 3.464101615137750834, 0.000000000000000000 ) ) ;
#3599 = DIRECTION ( 'NONE',  ( 0.000000000000000000, 0.000000000000000000, -1.000000000000000000 ) ) ;
#3600 = ADVANCED_FACE ( 'NONE', ( #14015 ), #10845, .F. ) ;
#3601 = ORIENTED_EDGE ( 'NONE', *, *, #5962, .F. ) ;
#3602 = CYLINDRICAL_SURFACE ( 'NONE', #12776, 2.649999999999985700 ) ;
#3603 = AXIS2_PLACEMENT_3D ( 'NONE', #2266, #2157, #11125 ) ;
#3604 = DIRECTION ( 'NONE',  ( 0.000000000000000000, 0.000000000000000000, -1.000000000000000000 ) ) ;
#3605 = CARTESIAN_POINT ( 'NONE',  ( 176.0000000000000000, 0.000000000000000000, 188.0000000000000000 ) ) ;
#3606 = ORIENTED_EDGE ( 'NONE', *, *, #10135, .T. ) ;
#3607 = DIRECTION ( 'NONE',  ( 0.000000000000000000, 0.000000000000000000, 1.000000000000000000 ) ) ;
#3608 = ORIENTED_EDGE ( 'NONE', *, *, #12502, .F. ) ;
#3609 = LINE ( 'NONE', #5576, #13441 ) ;
#3610 = AXIS2_PLACEMENT_3D ( 'NONE', #4855, #11445, #8024 ) ;
#3611 = ORIENTED_EDGE ( 'NONE', *, *, #2334, .T. ) ;
#3612 = ORIENTED_EDGE ( 'NONE', *, *, #13817, .F. ) ;
#3613 = DIRECTION ( 'NONE',  ( 1.000000000000000000, 0.000000000000000000, 0.000000000000000000 ) ) ;
#3614 = AXIS2_PLACEMENT_3D ( 'NONE', #4640, #9054, #12389 ) ;
#3615 = CARTESIAN_POINT ( 'NONE',  ( 1.287237434362044075, 3.875615274277557809, -3.430618716626812059 ) ) ;
#3616 = CARTESIAN_POINT ( 'NONE',  ( 124.9999999999999574, -64.99999999999997158, 10.00000000000000000 ) ) ;
#3617 = DIRECTION ( 'NONE',  ( -0.000000000000000000, -0.000000000000000000, -1.000000000000000000 ) ) ;
#3618 = DIRECTION ( 'NONE',  ( 0.000000000000000000, 0.000000000000000000, -1.000000000000000000 ) ) ;
#3619 = CARTESIAN_POINT ( 'NONE',  ( 2.500000000000000000, 0.000000000000000000, 0.000000000000000000 ) ) ;
#3620 = SURFACE_STYLE_FILL_AREA ( #12395 ) ;
#3621 = AXIS2_PLACEMENT_3D ( 'NONE', #13336, #5587, #14283 ) ;
#3622 = FACE_OUTER_BOUND ( 'NONE', #11623, .T. ) ;
#3623 = EDGE_CURVE ( 'NONE', #4356, #3798, #9295, .T. ) ;
#3624 = VECTOR ( 'NONE', #683, 1000.000000000000000 ) ;
#3625 = ORIENTED_EDGE ( 'NONE', *, *, #9490, .T. ) ;
#3626 = ORIENTED_EDGE ( 'NONE', *, *, #14034, .T. ) ;
#3627 = CIRCLE ( 'NONE', #8729, 5.000000000000004441 ) ;
#3628 = PLANE ( 'NONE',  #83 ) ;
#3629 = ORIENTED_EDGE ( 'NONE', *, *, #1415, .T. ) ;
#3630 = DIRECTION ( 'NONE',  ( -1.000000000000000000, -0.000000000000000000, -0.000000000000000000 ) ) ;
#3631 = AXIS2_PLACEMENT_3D ( 'NONE', #8951, #11347, #6987 ) ;
#3632 = ORIENTED_EDGE ( 'NONE', *, *, #11546, .F. ) ;
#3633 = CARTESIAN_POINT ( 'NONE',  ( 0.000000000000000000, 0.000000000000000000, -200.0000000000000000 ) ) ;
#3634 = ORIENTED_EDGE ( 'NONE', *, *, #13403, .F. ) ;
#3635 = CARTESIAN_POINT ( 'NONE',  ( -30.00000000000002842, -15.00000000000000000, 205.0000000000000284 ) ) ;
#3636 = DIRECTION ( 'NONE',  ( 0.000000000000000000, -2.664535259100375697E-15, -1.000000000000000000 ) ) ;
#3637 = EDGE_LOOP ( 'NONE', ( #2187, #8085 ) ) ;
#3638 = CARTESIAN_POINT ( 'NONE',  ( 119.9999999999999147, -25.00000000000000000, 169.9999999999999716 ) ) ;
#3639 = CIRCLE ( 'NONE', #598, 2.649999999999985700 ) ;
#3640 = FACE_OUTER_BOUND ( 'NONE', #6859, .T. ) ;
#3641 =( LENGTH_UNIT ( ) NAMED_UNIT ( * ) SI_UNIT ( .MILLI., .METRE. ) );
#3642 = CIRCLE ( 'NONE', #1318, 20.00000000000000000 ) ;
#3643 = CARTESIAN_POINT ( 'NONE',  ( 219.9999999999999716, -85.00000000000007105, 0.000000000000000000 ) ) ;
#3644 = EDGE_CURVE ( 'NONE', #566, #9071, #1913, .T. ) ;
#3645 = CARTESIAN_POINT ( 'NONE',  ( 134.9999999999999432, -56.99999999999997158, -154.9999999999999716 ) ) ;
#3646 = DIRECTION ( 'NONE',  ( 0.000000000000000000, 0.000000000000000000, -1.000000000000000000 ) ) ;
#3647 = AXIS2_PLACEMENT_3D ( 'NONE', #7773, #7708, #13725 ) ;
#3648 = VERTEX_POINT ( 'NONE', #2052 ) ;
#3649 = ORIENTED_EDGE ( 'NONE', *, *, #11650, .T. ) ;
#3650 = ORIENTED_EDGE ( 'NONE', *, *, #1694, .F. ) ;
#3651 = CARTESIAN_POINT ( 'NONE',  ( -30.00000000000002842, -20.00000000000000000, 200.0000000000000000 ) ) ;
#3652 = VECTOR ( 'NONE', #13453, 1000.000000000000000 ) ;
#3653 = CIRCLE ( 'NONE', #4820, 2.500000000000002220 ) ;
#3654 = ORIENTED_EDGE ( 'NONE', *, *, #7997, .F. ) ;
#3655 = DIRECTION ( 'NONE',  ( 0.000000000000000000, 1.000000000000000000, 0.000000000000000000 ) ) ;
#3656 = ORIENTED_EDGE ( 'NONE', *, *, #13239, .T. ) ;
#3657 = CARTESIAN_POINT ( 'NONE',  ( -5.000000000000000888, -8.660254037844389075, 199.9990000000000236 ) ) ;
#3658 = EDGE_CURVE ( 'NONE', #649, #13881, #3048, .T. ) ;
#3659 = EDGE_CURVE ( 'NONE', #7893, #2298, #11709, .T. ) ;
#3660 = CYLINDRICAL_SURFACE ( 'NONE', #11736, 2.649999999999985700 ) ;
#3661 = AXIS2_PLACEMENT_3D ( 'NONE', #11522, #9491, #12825 ) ;
#3662 = DIRECTION ( 'NONE',  ( 1.000000000000000000, 0.000000000000000000, 0.000000000000000000 ) ) ;
#3663 = EDGE_CURVE ( 'NONE', #6208, #67, #1835, .T. ) ;
#3664 =( GEOMETRIC_REPRESENTATION_CONTEXT ( 3 ) GLOBAL_UNCERTAINTY_ASSIGNED_CONTEXT ( ( #3870 ) ) GLOBAL_UNIT_ASSIGNED_CONTEXT ( ( #1848, #11794, #12015 ) ) REPRESENTATION_CONTEXT ( 'NONE', 'WORKASPACE' ) );
#3665 = DIRECTION ( 'NONE',  ( 0.000000000000000000, 0.000000000000000000, 1.000000000000000000 ) ) ;
#3666 = DIRECTION ( 'NONE',  ( 1.000000000000000000, 0.000000000000000000, 0.000000000000000000 ) ) ;
#3667 = VERTEX_POINT ( 'NONE', #3091 ) ;
#3668 = CIRCLE ( 'NONE', #11782, 2.041999999999999815 ) ;
#3669 = SURFACE_STYLE_USAGE ( .BOTH. , #4692 ) ;
#3670 = DIRECTION ( 'NONE',  ( -0.000000000000000000, -0.000000000000000000, 1.000000000000000000 ) ) ;
#3671 = DIRECTION ( 'NONE',  ( -1.000000000000000000, -0.000000000000000000, -0.000000000000000000 ) ) ;
#3672 = EDGE_CURVE ( 'NONE', #191, #8653, #928, .T. ) ;
#3673 = EDGE_CURVE ( 'NONE', #11569, #5871, #4671, .T. ) ;
#3674 = VECTOR ( 'NONE', #7788, 1000.000000000000000 ) ;
#3675 = ORIENTED_EDGE ( 'NONE', *, *, #12601, .T. ) ;
#3676 = PLANE ( 'NONE',  #8734 ) ;
#3677 = EDGE_CURVE ( 'NONE', #7302, #8946, #6520, .T. ) ;
#3678 = FACE_OUTER_BOUND ( 'NONE', #7255, .T. ) ;
#3679 = CARTESIAN_POINT ( 'NONE',  ( 136.6666666666666288, -30.00000000000000355, -222.5000000000000853 ) ) ;
#3680 = AXIS2_PLACEMENT_3D ( 'NONE', #2050, #8941, #3440 ) ;
#3681 = FACE_OUTER_BOUND ( 'NONE', #10157, .T. ) ;
#3682 = ORIENTED_EDGE ( 'NONE', *, *, #5797, .F. ) ;
#3683 = AXIS2_PLACEMENT_3D ( 'NONE', #5870, #13766, #317 ) ;
#3684 = CARTESIAN_POINT ( 'NONE',  ( 137.4999999999999432, -56.99999999999997158, -169.9999999999999716 ) ) ;
#3685 = PRODUCT_DEFINITION_SHAPE ( 'NONE', 'NONE',  #10925 ) ;
#3686 = DIRECTION ( 'NONE',  ( 1.000000000000000000, 0.000000000000000000, 0.000000000000000000 ) ) ;
#3687 = MANIFOLD_SOLID_BREP ( 'Hex', #11696 ) ;
#3688 = ORIENTED_EDGE ( 'NONE', *, *, #4327, .T. ) ;
#3689 = ORIENTED_EDGE ( 'NONE', *, *, #1610, .T. ) ;
#3690 = CARTESIAN_POINT ( 'NONE',  ( 386.6666666666666288, -20.00000000000000000, -219.8500000000001080 ) ) ;
#3691 = CARTESIAN_POINT ( 'NONE',  ( 0.000000000000000000, 0.000000000000000000, 4.000000000000000000 ) ) ;
#3692 = FACE_OUTER_BOUND ( 'NONE', #7470, .T. ) ;
#3693 = FACE_OUTER_BOUND ( 'NONE', #6504, .T. ) ;
#3694 = DIRECTION ( 'NONE',  ( 1.000000000000000000, 0.000000000000000000, 0.000000000000000000 ) ) ;
#3695 = FACE_OUTER_BOUND ( 'NONE', #13057, .T. ) ;
#3696 = VERTEX_POINT ( 'NONE', #6625 ) ;
#3697 = EDGE_CURVE ( 'NONE', #4582, #4565, #10914, .T. ) ;
#3698 = ORIENTED_EDGE ( 'NONE', *, *, #11535, .F. ) ;
#3699 = CARTESIAN_POINT ( 'NONE',  ( 119.9999999999999147, -20.00000000000000000, -169.9999999999999716 ) ) ;
#3700 = ORIENTED_EDGE ( 'NONE', *, *, #12163, .F. ) ;
#3701 = DIRECTION ( 'NONE',  ( 0.000000000000000000, 0.000000000000000000, 1.000000000000000000 ) ) ;
#3702 = AXIS2_PLACEMENT_3D ( 'NONE', #10551, #512, #2871 ) ;
#3703 = AXIS2_PLACEMENT_3D ( 'NONE', #10869, #10726, #2965 ) ;
#3704 = ORIENTED_EDGE ( 'NONE', *, *, #4998, .T. ) ;
#3705 = CARTESIAN_POINT ( 'NONE',  ( 239.1499999999999204, -85.00000000000007105, 50.00000000000001421 ) ) ;
#3706 = ORIENTED_EDGE ( 'NONE', *, *, #9692, .T. ) ;
#3707 = AXIS2_PLACEMENT_3D ( 'NONE', #602, #11876, #2886 ) ;
#3708 = DIRECTION ( 'NONE',  ( -0.000000000000000000, -0.000000000000000000, -1.000000000000000000 ) ) ;
#3709 = CARTESIAN_POINT ( 'NONE',  ( 319.9999999999999432, -20.00000000000000000, 19.99999999999998934 ) ) ;
#3710 = ORIENTED_EDGE ( 'NONE', *, *, #3219, .T. ) ;
#3711 = CIRCLE ( 'NONE', #11135, 10.00000000000000888 ) ;
#3712 = CARTESIAN_POINT ( 'NONE',  ( -5.000000000000000888, -8.660254037844389075, 210.0000000000000000 ) ) ;
#3713 = CARTESIAN_POINT ( 'NONE',  ( 140.0000000000000000, -95.00000000000008527, 186.2999999999999829 ) ) ;
#3714 = MANIFOLD_SOLID_BREP ( 'M5 Clearance Hole1', #2425 ) ;
#3715 = CARTESIAN_POINT ( 'NONE',  ( 2.500000000000000000, 2.357898499370433054, -1.951563910473907981E-15 ) ) ;
#3716 = VERTEX_POINT ( 'NONE', #1167 ) ;
#3717 = ORIENTED_EDGE ( 'NONE', *, *, #728, .T. ) ;
#3718 = ORIENTED_EDGE ( 'NONE', *, *, #5882, .T. ) ;
#3719 = DIRECTION ( 'NONE',  ( 1.000000000000000000, 0.000000000000000000, 0.000000000000000000 ) ) ;
#3720 = VERTEX_POINT ( 'NONE', #2345 ) ;
#3721 = DIRECTION ( 'NONE',  ( -0.000000000000000000, -0.000000000000000000, 1.000000000000000000 ) ) ;
#3722 = EDGE_LOOP ( 'NONE', ( #7661, #13068, #6269, #1884 ) ) ;
#3723 = ADVANCED_FACE ( 'NONE', ( #12205 ), #958, .F. ) ;
#3724 = FACE_BOUND ( 'NONE', #323, .T. ) ;
#3725 = EDGE_CURVE ( 'NONE', #2417, #4230, #1852, .T. ) ;
#3726 = CARTESIAN_POINT ( 'NONE',  ( 181.0000000000000000, 8.660254037844390851, 200.0000000000000000 ) ) ;
#3727 = LINE ( 'NONE', #9923, #2004 ) ;
#3728 = CARTESIAN_POINT ( 'NONE',  ( 386.6666666666666288, -25.00000000000000000, 222.5000000000000853 ) ) ;
#3729 = VECTOR ( 'NONE', #4243, 1000.000000000000000 ) ;
#3730 = CYLINDRICAL_SURFACE ( 'NONE', #6968, 5.500000000000005329 ) ;
#3731 = CARTESIAN_POINT ( 'NONE',  ( -307.6499999999999204, 45.00000000000001421, 30.00000000000000000 ) ) ;
#3732 = DIRECTION ( 'NONE',  ( -1.000000000000000000, -0.000000000000000000, -0.000000000000000000 ) ) ;
#3733 = EDGE_CURVE ( 'NONE', #1448, #1006, #3027, .T. ) ;
#3734 = VERTEX_POINT ( 'NONE', #8943 ) ;
#3735 = AXIS2_PLACEMENT_3D ( 'NONE', #5207, #9622, #2072 ) ;
#3736 = PRESENTATION_LAYER_ASSIGNMENT (  '', '', ( #13038 ) ) ;
#3737=STYLED_ITEM('',(#14417),#3853);
#3738 = CARTESIAN_POINT ( 'NONE',  ( 1.794155980045911036, 5.817072295949926440E-16, -4.749999999999999112 ) ) ;
#3739 = EDGE_CURVE ( 'NONE', #12934, #6489, #13956, .T. ) ;
#3740 = LINE ( 'NONE', #8153, #12568 ) ;
#3741 = ADVANCED_FACE ( 'NONE', ( #3304 ), #10989, .F. ) ;
#3742 = PLANE ( 'NONE',  #11775 ) ;
#3743 = ORIENTED_EDGE ( 'NONE', *, *, #4638, .T. ) ;
#3744 = AXIS2_PLACEMENT_3D ( 'NONE', #5000, #13836, #6082 ) ;
#3745 = CARTESIAN_POINT ( 'NONE',  ( 236.4999999999999432, -85.00000000000007105, 55.00000000000001421 ) ) ;
#3746 = AXIS2_PLACEMENT_3D ( 'NONE', #3121, #3403, #7802 ) ;
#3747 = DIRECTION ( 'NONE',  ( -0.000000000000000000, 1.000000000000000000, 1.224646799147353207E-16 ) ) ;
#3748 = DIRECTION ( 'NONE',  ( 0.000000000000000000, 0.000000000000000000, 1.000000000000000000 ) ) ;
#3749 = EDGE_CURVE ( 'NONE', #11189, #9294, #5931, .T. ) ;
#3750 = CARTESIAN_POINT ( 'NONE',  ( 2.500000000000000000, 2.629050547790028946E-15, 2.042000000000000259 ) ) ;
#3751 = ADVANCED_FACE ( 'NONE', ( #10098 ), #13426, .F. ) ;
#3752 = EDGE_CURVE ( 'NONE', #5974, #11887, #5463, .T. ) ;
#3753 = EDGE_CURVE ( 'NONE', #8807, #2351, #8878, .T. ) ;
#3754 = EDGE_CURVE ( 'NONE', #11555, #2842, #12350, .T. ) ;
#3755 = ORIENTED_EDGE ( 'NONE', *, *, #9883, .T. ) ;
#3756 = CARTESIAN_POINT ( 'NONE',  ( 144.9999999999999716, -64.99999999999997158, 10.00000000000000000 ) ) ;
#3757 = CIRCLE ( 'NONE', #9562, 2.649999999999985700 ) ;
#3758 = CARTESIAN_POINT ( 'NONE',  ( 5.200000000000002842, 0.000000000000000000, 0.000000000000000000 ) ) ;
#3759 = ADVANCED_FACE ( 'NONE', ( #4310 ), #13153, .F. ) ;
#3760 = AXIS2_PLACEMENT_3D ( 'NONE', #9555, #12955, #9404 ) ;
#3761 = ORIENTED_EDGE ( 'NONE', *, *, #5646, .F. ) ;
#3762 = CIRCLE ( 'NONE', #7689, 2.649999999999985700 ) ;
#3763 = CARTESIAN_POINT ( 'NONE',  ( 219.9999999999999716, -15.00000000000000000, 222.5000000000000853 ) ) ;
#3764 = CARTESIAN_POINT ( 'NONE',  ( -124.9999999999999432, 55.00000000000001421, 30.00000000000000000 ) ) ;
#3765 = DIRECTION ( 'NONE',  ( -0.000000000000000000, 1.000000000000000000, 1.224646799147353207E-16 ) ) ;
#3766 = DIRECTION ( 'NONE',  ( -1.000000000000000000, -2.478176394252579230E-17, -0.000000000000000000 ) ) ;
#3767 = CARTESIAN_POINT ( 'NONE',  ( 347.0000000000000000, 8.660254037844390851, 200.0000000000000000 ) ) ;
#3768 = FILL_AREA_STYLE_COLOUR ( '', #10709 ) ;
#3769 = AXIS2_PLACEMENT_3D ( 'NONE', #11136, #1178, #5619 ) ;
#3770 = DIRECTION ( 'NONE',  ( 1.000000000000000000, 0.000000000000000000, 0.000000000000000000 ) ) ;
#3771 = PRODUCT_DEFINITION_FORMATION_WITH_SPECIFIED_SOURCE ( 'ANY', '', #11441, .NOT_KNOWN. ) ;
#3772 = VERTEX_POINT ( 'NONE', #13785 ) ;
#3773 = COLOUR_RGB ( '',0.8941176470588234615, 0.8941176470588234615, 0.8941176470588234615 ) ;
#3774 = VERTEX_POINT ( 'NONE', #6031 ) ;
#3775 = DIRECTION ( 'NONE',  ( 1.000000000000000000, 0.000000000000000000, 0.000000000000000000 ) ) ;
#3776 = ORIENTED_EDGE ( 'NONE', *, *, #1064, .T. ) ;
#3777 = CARTESIAN_POINT ( 'NONE',  ( 4.024499207728847949, -2.323545700935699454, -3.572172305156873673 ) ) ;
#3778 = DIRECTION ( 'NONE',  ( 1.000000000000000000, 0.000000000000000000, 0.000000000000000000 ) ) ;
#3779 = VECTOR ( 'NONE', #5752, 1000.000000000000000 ) ;
#3780 = EDGE_LOOP ( 'NONE', ( #12090, #6328, #7485, #8984 ) ) ;
#3781 = CARTESIAN_POINT ( 'NONE',  ( 302.6499999999999204, -95.00000000000008527, -186.2999999999999829 ) ) ;
#3782 = ORIENTED_EDGE ( 'NONE', *, *, #7821, .F. ) ;
#3783 = DIRECTION ( 'NONE',  ( -0.000000000000000000, 1.000000000000000000, -0.000000000000000000 ) ) ;
#3784 = DIRECTION ( 'NONE',  ( 0.000000000000000000, 0.000000000000000000, -1.000000000000000000 ) ) ;
#3785 = ORIENTED_EDGE ( 'NONE', *, *, #12600, .F. ) ;
#3786 = CARTESIAN_POINT ( 'NONE',  ( 2.740000000000000213, 0.5150000000000024558, -0.6774776749089207462 ) ) ;
#3787 = EDGE_CURVE ( 'NONE', #5325, #2741, #4445, .T. ) ;
#3788 = CARTESIAN_POINT ( 'NONE',  ( 219.9999999999999716, -20.00000000000000000, 222.5000000000000853 ) ) ;
#3789 = SHAPE_DEFINITION_REPRESENTATION ( #9119, #2275 ) ;
#3790 = DIRECTION ( 'NONE',  ( -1.000000000000000000, 0.000000000000000000, 0.000000000000000000 ) ) ;
#3791 = EDGE_LOOP ( 'NONE', ( #12631, #5458, #6276 ) ) ;
#3792 = ORIENTED_EDGE ( 'NONE', *, *, #8052, .F. ) ;
#3793 = B_SPLINE_CURVE_WITH_KNOTS ( 'NONE', 3,
 ( #13799, #3800, #6121, #4087, #8510, #13947, #4023, #10398 ),
 .UNSPECIFIED., .F., .F.,
 ( 4, 2, 2, 4 ),
 ( 7.780516681398759253E-20, 0.002450665683189819696, 0.003675998524784729327, 0.004901331366379639391 ),
 .UNSPECIFIED. ) ;
#3794 = EDGE_LOOP ( 'NONE', ( #12275, #2354, #2420, #13391 ) ) ;
#3795 = DIRECTION ( 'NONE',  ( 1.000000000000000000, 0.000000000000000000, -0.000000000000000000 ) ) ;
#3796 = ORIENTED_EDGE ( 'NONE', *, *, #6767, .F. ) ;
#3797 = DIRECTION ( 'NONE',  ( 1.000000000000000000, 0.000000000000000000, 0.000000000000000000 ) ) ;
#3798 = VERTEX_POINT ( 'NONE', #11336 ) ;
#3799 = LINE ( 'NONE', #9315, #10831 ) ;
#3800 = CARTESIAN_POINT ( 'NONE',  ( 0.6920835326022565237, 4.454600218803884459, -3.597382984111579862 ) ) ;
#3801 = DIRECTION ( 'NONE',  ( 0.000000000000000000, 0.000000000000000000, 1.000000000000000000 ) ) ;
#3802 = DIRECTION ( 'NONE',  ( 0.000000000000000000, -1.000000000000000000, 0.000000000000000000 ) ) ;
#3803 = PLANE ( 'NONE',  #4842 ) ;
#3804 = PRODUCT_DEFINITION_SHAPE ( 'NONE', 'NONE',  #14366 ) ;
#3805 = ORIENTED_EDGE ( 'NONE', *, *, #3399, .F. ) ;
#3806 = EDGE_CURVE ( 'NONE', #6489, #9721, #4883, .T. ) ;
#3807 = ORIENTED_EDGE ( 'NONE', *, *, #3739, .T. ) ;
#3808 = DIRECTION ( 'NONE',  ( -0.000000000000000000, -0.000000000000000000, 1.000000000000000000 ) ) ;
#3809 = DIRECTION ( 'NONE',  ( -0.000000000000000000, -0.000000000000000000, -1.000000000000000000 ) ) ;
#3810 = CLOSED_SHELL ( 'NONE', ( #7980, #528, #10284, #12528, #450, #11788, #1879, #11864, #12453, #9342, #5261, #6691, #9234, #1174, #4628, #13130, #91, #6937, #10572, #13117, #413, #6012, #13880, #14110 ) ) ;
#3811 = LINE ( 'NONE', #6425, #4363 ) ;
#3812 = ORIENTED_EDGE ( 'NONE', *, *, #11890, .T. ) ;
#3813 = CYLINDRICAL_SURFACE ( 'NONE', #8603, 2.500000000000000444 ) ;
#3814 = DIRECTION ( 'NONE',  ( 0.000000000000000000, 1.000000000000000000, 0.000000000000000000 ) ) ;
#3815 = DIRECTION ( 'NONE',  ( 1.000000000000000000, 0.000000000000000000, 0.000000000000000000 ) ) ;
#3816 = CARTESIAN_POINT ( 'NONE',  ( 119.9999999999999147, -24.99999999999999289, -19.99999999999998934 ) ) ;
#3817 = EDGE_CURVE ( 'NONE', #11952, #10315, #3711, .T. ) ;
#3818 = CYLINDRICAL_SURFACE ( 'NONE', #10112, 2.649999999999985700 ) ;
#3819 = PRODUCT_DEFINITION ( 'UNKNOWN', '', #2382, #6290 ) ;
#3820 = EDGE_LOOP ( 'NONE', ( #3204, #2586, #4776, #4282 ) ) ;
#3821 = CARTESIAN_POINT ( 'NONE',  ( -0.6448876103708541807, -4.246476118072358474, -0.2256878752776773356 ) ) ;
#3822 = CARTESIAN_POINT ( 'NONE',  ( 299.9999999999999432, -95.00000000000008527, -190.0000000000000000 ) ) ;
#3823 = MANIFOLD_SOLID_BREP ( 'AdvancedHole2', #5223 ) ;
#3824 = ORIENTED_EDGE ( 'NONE', *, *, #758, .F. ) ;
#3825 = DIRECTION ( 'NONE',  ( -1.000000000000000000, -0.000000000000000000, -0.000000000000000000 ) ) ;
#3826 = ADVANCED_FACE ( 'NONE', ( #3575 ), #205, .T. ) ;
#3827 = ADVANCED_FACE ( 'NONE', ( #8055 ), #5960, .F. ) ;
#3828 = CONICAL_SURFACE ( 'NONE', #10086, 0.8509999999999999787, 0.06981317007976602096 ) ;
#3829 = LINE ( 'NONE', #6006, #3407 ) ;
#3830 = EDGE_CURVE ( 'NONE', #3844, #5376, #4955, .T. ) ;
#3831 = DIRECTION ( 'NONE',  ( -1.000000000000000000, 0.000000000000000000, -0.000000000000000000 ) ) ;
#3832 = SHAPE_REPRESENTATION ( 'side rail', ( #14039 ), #3087 ) ;
#3833 = LINE ( 'NONE', #7029, #5605 ) ;
#3834 = DIRECTION ( 'NONE',  ( -1.000000000000000000, -0.000000000000000000, -0.000000000000000000 ) ) ;
#3835 =( NAMED_UNIT ( * ) SI_UNIT ( $, .STERADIAN. ) SOLID_ANGLE_UNIT ( ) );
#3836 = DIRECTION ( 'NONE',  ( 0.000000000000000000, 0.000000000000000000, -1.000000000000000000 ) ) ;
#3837 = ORIENTED_EDGE ( 'NONE', *, *, #8504, .T. ) ;
#3838 = CARTESIAN_POINT ( 'NONE',  ( 2.740000000000000213, 0.000000000000000000, 0.000000000000000000 ) ) ;
#3839 = EDGE_LOOP ( 'NONE', ( #12883, #2733, #2776, #4531, #6437, #13295, #2231 ) ) ;
#3840 = DIRECTION ( 'NONE',  ( -0.000000000000000000, 0.000000000000000000, 1.000000000000000000 ) ) ;
#3841 = CARTESIAN_POINT ( 'NONE',  ( 0.000000000000000000, 0.000000000000000000, 190.0000000000000000 ) ) ;
#3842 = ORIENTED_EDGE ( 'NONE', *, *, #3318, .F. ) ;
#3843 = CARTESIAN_POINT ( 'NONE',  ( -0.6937372685066653943, 4.453844082567723461, -3.610536846335889116 ) ) ;
#3844 = VERTEX_POINT ( 'NONE', #8275 ) ;
#3845 = CARTESIAN_POINT ( 'NONE',  ( 0.9586399445693646326, 0.8293189044373081575, 0.5149999999999996803 ) ) ;
#3846 = LINE ( 'NONE', #13498, #2957 ) ;
#3847 = ORIENTED_EDGE ( 'NONE', *, *, #2758, .T. ) ;
#3848 = EDGE_CURVE ( 'NONE', #1662, #5504, #8130, .T. ) ;
#3849 = DIRECTION ( 'NONE',  ( 1.000000000000000000, 0.000000000000000000, 0.000000000000000000 ) ) ;
#3850 = DIRECTION ( 'NONE',  ( 0.000000000000000000, -1.000000000000000000, -1.652937667529658626E-16 ) ) ;
#3851 = AXIS2_PLACEMENT_3D ( 'NONE', #2987, #13120, #3205 ) ;
#3852 = SURFACE_SIDE_STYLE ('',( #12488 ) ) ;
#3853 = MANIFOLD_SOLID_BREP ( 'Hex', #12850 ) ;
#3854 = CARTESIAN_POINT ( 'NONE',  ( 0.000000000000000000, 1.178949249685212974, -2.042000000000001148 ) ) ;
#3855 = APPLICATION_PROTOCOL_DEFINITION ( 'draft international standard', 'automotive_design', 1998, #605 ) ;
#3856 = AXIS2_PLACEMENT_3D ( 'NONE', #6707, #1181, #6569 ) ;
#3857 = DIRECTION ( 'NONE',  ( 1.000000000000000000, 0.000000000000000000, 0.000000000000000000 ) ) ;
#3858 = ORIENTED_EDGE ( 'NONE', *, *, #8825, .F. ) ;
#3859 = ORIENTED_EDGE ( 'NONE', *, *, #12953, .F. ) ;
#3860 = VECTOR ( 'NONE', #13064, 1000.000000000000000 ) ;
#3861 = EDGE_LOOP ( 'NONE', ( #13502, #1650, #12377, #6158 ) ) ;
#3862 = EDGE_CURVE ( 'NONE', #4077, #11692, #9149, .T. ) ;
#3863 = PLANE ( 'NONE',  #13468 ) ;
#3864 = CIRCLE ( 'NONE', #11976, 2.649999999999985700 ) ;
#3865 = TOROIDAL_SURFACE ( 'NONE', #349, 2.700000000000000622, 0.2000000000000000111 ) ;
#3866 = EDGE_LOOP ( 'NONE', ( #8353, #118, #8905 ) ) ;
#3867 = CARTESIAN_POINT ( 'NONE',  ( 1.999999999999994893, 1.313433692085536476E-15, 10.72499999999999964 ) ) ;
#3868 = ORIENTED_EDGE ( 'NONE', *, *, #3309, .F. ) ;
#3869 = DIRECTION ( 'NONE',  ( -1.000000000000000000, 0.000000000000000000, 0.000000000000000000 ) ) ;
#3870 = UNCERTAINTY_MEASURE_WITH_UNIT (LENGTH_MEASURE( 1.000000000000000082E-05 ), #1848, 'distance_accuracy_value', 'NONE');
#3871 = CARTESIAN_POINT ( 'NONE',  ( 0.000000000000000000, 2.357898499370433054, -1.951563910473907981E-15 ) ) ;
#3872 = FACE_OUTER_BOUND ( 'NONE', #6127, .T. ) ;
#3873 = AXIS2_PLACEMENT_3D ( 'NONE', #10361, #6953, #5935 ) ;
#3874 = APPLICATION_CONTEXT ( 'automotive_design' ) ;
#3875 = DIRECTION ( 'NONE',  ( -0.000000000000000000, -0.000000000000000000, 1.000000000000000000 ) ) ;
#3876 = DIRECTION ( 'NONE',  ( -0.000000000000000000, -0.000000000000000000, -1.000000000000000000 ) ) ;
#3877 = LINE ( 'NONE', #4090, #7803 ) ;
#3878 = ORIENTED_EDGE ( 'NONE', *, *, #5281, .T. ) ;
#3879 = VECTOR ( 'NONE', #11827, 1000.000000000000000 ) ;
#3880 = EDGE_LOOP ( 'NONE', ( #7690, #5200 ) ) ;
#3881 = AXIS2_PLACEMENT_3D ( 'NONE', #5954, #1586, #4735 ) ;
#3882 = MANIFOLD_SOLID_BREP ( 'AdvancedHole1', #12608 ) ;
#3883 = EDGE_CURVE ( 'NONE', #4614, #5679, #12996, .T. ) ;
#3884 =( NAMED_UNIT ( * ) PLANE_ANGLE_UNIT ( ) SI_UNIT ( $, .RADIAN. ) );
#3885 = ORIENTED_EDGE ( 'NONE', *, *, #6936, .F. ) ;
#3886 = CARTESIAN_POINT ( 'NONE',  ( 1.655952806101427033, -3.662737355149048302, -1.182683869819604841E-14 ) ) ;
#3887 = CARTESIAN_POINT ( 'NONE',  ( 170.9999999999999716, 8.660254037844390851, 205.0000000000000284 ) ) ;
#3888 = AXIS2_PLACEMENT_3D ( 'NONE', #6533, #14211, #7819 ) ;
#3889 = DIRECTION ( 'NONE',  ( 0.000000000000000000, 1.000000000000000000, 0.000000000000000000 ) ) ;
#3890 = ORIENTED_EDGE ( 'NONE', *, *, #5593, .T. ) ;
#3891 = EDGE_CURVE ( 'NONE', #8759, #8867, #10221, .T. ) ;
#3892 = MECHANICAL_DESIGN_GEOMETRIC_PRESENTATION_REPRESENTATION (  '', ( #13607 ), #11305 ) ;
#3893 = DIRECTION ( 'NONE',  ( 1.000000000000000000, 0.000000000000000000, 0.000000000000000000 ) ) ;
#3894 = CARTESIAN_POINT ( 'NONE',  ( 0.3226060873438383325, 0.5149999999999923528, 2.189154565102733319 ) ) ;
#3895 = CARTESIAN_POINT ( 'NONE',  ( 299.9999999999999432, -95.00000000000008527, -190.0000000000000000 ) ) ;
#3896 = DIRECTION ( 'NONE',  ( -0.000000000000000000, -0.000000000000000000, 1.000000000000000000 ) ) ;
#3897 = DIRECTION ( 'NONE',  ( -0.000000000000000000, 1.000000000000000000, -0.000000000000000000 ) ) ;
#3898 = ORIENTED_EDGE ( 'NONE', *, *, #6140, .T. ) ;
#3899 = COLOUR_RGB ( '',0.8941176470588234615, 0.8941176470588234615, 0.8941176470588234615 ) ;
#3900 = DIRECTION ( 'NONE',  ( -0.000000000000000000, -1.000000000000000000, -0.000000000000000000 ) ) ;
#3901 = FACE_BOUND ( 'NONE', #4803, .T. ) ;
#3902 = ORIENTED_EDGE ( 'NONE', *, *, #3404, .F. ) ;
#3904 = ADVANCED_FACE ( 'NONE', ( #11688 ), #12777, .F. ) ;
#3903 = CARTESIAN_POINT ( 'NONE',  ( -30.00000000000000000, 0.000000000000000000, 200.0000000000000000 ) ) ;
#3905 = ADVANCED_FACE ( 'NONE', ( #10611 ), #11586, .T. ) ;
#3906 = CARTESIAN_POINT ( 'NONE',  ( 0.000000000000000000, 0.5150000000000083400, -2.349999999999997424 ) ) ;
#3907 = CIRCLE ( 'NONE', #1112, 0.8509999999999999787 ) ;
#3908 = CARTESIAN_POINT ( 'NONE',  ( 236.4999999999999432, -85.00000000000007105, 55.00000000000001421 ) ) ;
#3909 = DIRECTION ( 'NONE',  ( -0.5000000000000019984, -0.8660254037844375974, 0.000000000000000000 ) ) ;
#3910 = CARTESIAN_POINT ( 'NONE',  ( 170.9999999999999716, 8.660254037844390851, 205.0000000000000284 ) ) ;
#3911 = PRESENTATION_STYLE_ASSIGNMENT (( #8547 ) ) ;
#3912 = CARTESIAN_POINT ( 'NONE',  ( 4.000000000000000888, 1.563622288139206118, -0.2253451193528334950 ) ) ;
#3913 = EDGE_LOOP ( 'NONE', ( #10279, #3163, #3608, #6475 ) ) ;
#3914 = EDGE_CURVE ( 'NONE', #7589, #12061, #9591, .T. ) ;
#3915 = CARTESIAN_POINT ( 'NONE',  ( -217.3499999999999375, -85.00000000000009948, 30.00000000000000000 ) ) ;
#3916 = CIRCLE ( 'NONE', #10874, 2.649999999999985700 ) ;
#3917 = EDGE_LOOP ( 'NONE', ( #4509, #10710, #10725, #9876 ) ) ;
#3918 = DIRECTION ( 'NONE',  ( -0.000000000000000000, -0.000000000000000000, -1.000000000000000000 ) ) ;
#3919 = DIRECTION ( 'NONE',  ( -1.000000000000000000, -0.000000000000000000, -0.000000000000000000 ) ) ;
#3920 = VERTEX_POINT ( 'NONE', #4004 ) ;
#3921 = CARTESIAN_POINT ( 'NONE',  ( -4.207491450040567571, 2.029819825146470524, -3.671670828759566074 ) ) ;
#3922 = ORIENTED_EDGE ( 'NONE', *, *, #2818, .F. ) ;
#3923 = VECTOR ( 'NONE', #10273, 1000.000000000000000 ) ;
#3925 = EDGE_CURVE ( 'NONE', #13016, #7650, #4072, .T. ) ;
#3924 = DIRECTION ( 'NONE',  ( -1.000000000000000000, -0.000000000000000000, -0.000000000000000000 ) ) ;
#3926 = PRODUCT_DEFINITION_SHAPE ( 'NONE', 'NONE',  #14363 ) ;
#3927 = DIRECTION ( 'NONE',  ( 0.000000000000000000, 0.000000000000000000, 1.000000000000000000 ) ) ;
#3928 = ORIENTED_EDGE ( 'NONE', *, *, #7805, .T. ) ;
#3929 = FACE_BOUND ( 'NONE', #7921, .T. ) ;
#3930 = CARTESIAN_POINT ( 'NONE',  ( 2.500000000000000000, 0.000000000000000000, 0.000000000000000000 ) ) ;
#3931 = FACE_OUTER_BOUND ( 'NONE', #13592, .T. ) ;
#3932 = APPLICATION_PROTOCOL_DEFINITION ( 'draft international standard', 'automotive_design', 1998, #5635 ) ;
#3933 = DIRECTION ( 'NONE',  ( 1.000000000000000000, 0.000000000000000000, 0.000000000000000000 ) ) ;
#3934 = EDGE_LOOP ( 'NONE', ( #115, #6026 ) ) ;
#3935 = AXIS2_PLACEMENT_3D ( 'NONE', #7654, #9770, #12149 ) ;
#3936 = ORIENTED_EDGE ( 'NONE', *, *, #7699, .F. ) ;
#3937 = ADVANCED_FACE ( 'NONE', ( #6247 ), #2915, .F. ) ;
#3938 = DIRECTION ( 'NONE',  ( -1.000000000000000000, 0.000000000000000000, 0.000000000000000000 ) ) ;
#3939 = ORIENTED_EDGE ( 'NONE', *, *, #5202, .T. ) ;
#3940 = CIRCLE ( 'NONE', #12049, 2.500000000000001332 ) ;
#3941 = ADVANCED_FACE ( 'NONE', ( #3931 ), #8488, .T. ) ;
#3942 = CIRCLE ( 'NONE', #10186, 2.649999999999985700 ) ;
#3943 = CARTESIAN_POINT ( 'NONE',  ( 4.999999999999999112, 8.660254037844390851, -210.0000000000000000 ) ) ;
#3944 = ORIENTED_EDGE ( 'NONE', *, *, #9760, .T. ) ;
#3945 = ORIENTED_EDGE ( 'NONE', *, *, #1947, .T. ) ;
#3946 = DIRECTION ( 'NONE',  ( 1.000000000000000000, 0.000000000000000000, 0.000000000000000000 ) ) ;
#3947 = ADVANCED_FACE ( 'NONE', ( #10823, #9736 ), #3140, .T. ) ;
#3948 = CARTESIAN_POINT ( 'NONE',  ( 145.5000000000000284, -75.00000000000008527, -186.2999999999999829 ) ) ;
#3949 = DIRECTION ( 'NONE',  ( 0.000000000000000000, 0.000000000000000000, 1.000000000000000000 ) ) ;
#3950 = CARTESIAN_POINT ( 'NONE',  ( 1.567478505476134606E-15, 4.618802153517012066, -5.000000000000000000 ) ) ;
#3951 = CIRCLE ( 'NONE', #5791, 2.041999999999999815 ) ;
#3952 = DIRECTION ( 'NONE',  ( -0.000000000000000000, -0.000000000000000000, -1.000000000000000000 ) ) ;
#3953 = DIRECTION ( 'NONE',  ( -0.000000000000000000, -0.000000000000000000, -1.000000000000000000 ) ) ;
#3954 = VERTEX_POINT ( 'NONE', #8344 ) ;
#3955 = CONICAL_SURFACE ( 'NONE', #8589, 0.8509999999999999787, 0.06981317007976602096 ) ;
#3956 = ORIENTED_EDGE ( 'NONE', *, *, #12842, .F. ) ;
#3957 = DIRECTION ( 'NONE',  ( 0.000000000000000000, -1.000000000000000000, 0.000000000000000000 ) ) ;
#3958 = VERTEX_POINT ( 'NONE', #12185 ) ;
#3959 = DIRECTION ( 'NONE',  ( 0.000000000000000000, 0.000000000000000000, 1.000000000000000000 ) ) ;
#3960 = PLANE ( 'NONE',  #10247 ) ;
#3961 = ORIENTED_EDGE ( 'NONE', *, *, #1323, .T. ) ;
#3962 = VECTOR ( 'NONE', #7209, 1000.000000000000000 ) ;
#3963 = FACE_BOUND ( 'NONE', #14205, .T. ) ;
#3964 = EDGE_CURVE ( 'NONE', #13344, #5408, #3282, .T. ) ;
#3965 = DIRECTION ( 'NONE',  ( 1.000000000000000000, 0.000000000000000000, 0.000000000000000000 ) ) ;
#3966 = DIRECTION ( 'NONE',  ( 0.000000000000000000, 0.000000000000000000, -1.000000000000000000 ) ) ;
#3967 = AXIS2_PLACEMENT_3D ( 'NONE', #13098, #14117, #9632 ) ;
#3968 = FACE_OUTER_BOUND ( 'NONE', #11961, .T. ) ;
#3969 = AXIS2_PLACEMENT_3D ( 'NONE', #6325, #5314, #5024 ) ;
#3970 = ORIENTED_EDGE ( 'NONE', *, *, #11906, .F. ) ;
#3971 = DIRECTION ( 'NONE',  ( -1.000000000000000000, 0.000000000000000000, 0.000000000000000000 ) ) ;
#3972 = PLANE ( 'NONE',  #9753 ) ;
#3973 = CIRCLE ( 'NONE', #7213, 2.041999999999999815 ) ;
#3974 = EDGE_LOOP ( 'NONE', ( #2989, #5661, #9764, #10731 ) ) ;
#3975 = LINE ( 'NONE', #10734, #596 ) ;
#3976 =( GEOMETRIC_REPRESENTATION_CONTEXT ( 3 ) GLOBAL_UNCERTAINTY_ASSIGNED_CONTEXT ( ( #5511 ) ) GLOBAL_UNIT_ASSIGNED_CONTEXT ( ( #6883, #10289, #8397 ) ) REPRESENTATION_CONTEXT ( 'NONE', 'WORKASPACE' ) );
#3977 = EDGE_CURVE ( 'NONE', #7393, #1896, #3489, .T. ) ;
#3978 = SURFACE_SIDE_STYLE ('',( #538 ) ) ;
#3979 = PRESENTATION_STYLE_ASSIGNMENT (( #2823 ) ) ;
#3980 = CARTESIAN_POINT ( 'NONE',  ( -2.804994570502171047, -3.229033611042465335, -3.526374918436838701 ) ) ;
#3981 = CARTESIAN_POINT ( 'NONE',  ( 0.000000000000000000, 0.000000000000000000, 200.0000000000000000 ) ) ;
#3982 = FACE_BOUND ( 'NONE', #280, .T. ) ;
#3983 = CARTESIAN_POINT ( 'NONE',  ( -0.6640947660597427138, 4.471078309994878985, -3.602146406945963442 ) ) ;
#3984 = VECTOR ( 'NONE', #5654, 1000.000000000000000 ) ;
#3985 = ORIENTED_EDGE ( 'NONE', *, *, #8012, .F. ) ;
#3986 = EDGE_CURVE ( 'NONE', #6598, #13972, #13276, .T. ) ;
#3987 = PLANE ( 'NONE',  #12167 ) ;
#3988 = EDGE_CURVE ( 'NONE', #10103, #9376, #3358, .T. ) ;
#3989 = EDGE_LOOP ( 'NONE', ( #9097, #319, #9195, #6339 ) ) ;
#3990 = AXIS2_PLACEMENT_3D ( 'NONE', #9744, #5389, #10903 ) ;
#3991 = CARTESIAN_POINT ( 'NONE',  ( -1.800000000000001155, 0.000000000000000000, -13.29999999999999893 ) ) ;
#3992 = CARTESIAN_POINT ( 'NONE',  ( -31.74999999999995737, 0.000000000000000000, 2.500000000000000888 ) ) ;
#3993 = VERTEX_POINT ( 'NONE', #11038 ) ;
#3994 = DIRECTION ( 'NONE',  ( -0.000000000000000000, -0.000000000000000000, -1.000000000000000000 ) ) ;
#3995 = ORIENTED_EDGE ( 'NONE', *, *, #8942, .F. ) ;
#3996 = FACE_OUTER_BOUND ( 'NONE', #4248, .T. ) ;
#3997 = DIRECTION ( 'NONE',  ( -1.000000000000000000, 0.000000000000000000, 0.000000000000000000 ) ) ;
#3998 = ORIENTED_EDGE ( 'NONE', *, *, #11443, .T. ) ;
#3999 = CARTESIAN_POINT ( 'NONE',  ( 302.5000000000000000, -36.99999999999997868, -169.9999999999999716 ) ) ;
#4000 = FACE_OUTER_BOUND ( 'NONE', #3514, .T. ) ;
#4001 = ORIENTED_EDGE ( 'NONE', *, *, #9152, .F. ) ;
#4002 =( LENGTH_UNIT ( ) NAMED_UNIT ( * ) SI_UNIT ( .MILLI., .METRE. ) );
#4003 = STYLED_ITEM ( 'NONE', ( #12442 ), #1054 ) ;
#4004 = CARTESIAN_POINT ( 'NONE',  ( -2.499999999999999556, 3.061616997868382648E-16, 3.469446951953614189E-15 ) ) ;
#4005 = ITEM_DEFINED_TRANSFORMATION ( 'NONE', 'NONE', #10007,  #14039 ) ;
#4006 = CARTESIAN_POINT ( 'NONE',  ( 219.9999999999999147, -85.00000000000009948, -17.55500000000000327 ) ) ;
#4007 = VERTEX_POINT ( 'NONE', #10895 ) ;
#4008 =( REPRESENTATION_RELATIONSHIP ('NONE','NONE', #11251, #10314 ) REPRESENTATION_RELATIONSHIP_WITH_TRANSFORMATION ( #13259 )SHAPE_REPRESENTATION_RELATIONSHIP( ) );
#4009 = ORIENTED_EDGE ( 'NONE', *, *, #3498, .T. ) ;
#4010 = ADVANCED_FACE ( 'NONE', ( #920 ), #6681, .F. ) ;
#4011 = ORIENTED_EDGE ( 'NONE', *, *, #13229, .T. ) ;
#4012 = ADVANCED_FACE ( 'NONE', ( #1069 ), #48, .F. ) ;
#4013 = AXIS2_PLACEMENT_3D ( 'NONE', #882, #7437, #4253 ) ;
#4014 = ORIENTED_EDGE ( 'NONE', *, *, #13714, .F. ) ;
#4015 = LINE ( 'NONE', #7129, #10195 ) ;
#4016 = ORIENTED_EDGE ( 'NONE', *, *, #3152, .F. ) ;
#4017 = ORIENTED_EDGE ( 'NONE', *, *, #13817, .T. ) ;
#4018 = DIRECTION ( 'NONE',  ( -0.000000000000000000, -0.000000000000000000, 1.000000000000000000 ) ) ;
#4019 = ORIENTED_EDGE ( 'NONE', *, *, #5003, .T. ) ;
#4020 = CARTESIAN_POINT ( 'NONE',  ( -5.000000000000000888, 8.660254037844390851, 205.0000000000000284 ) ) ;
#4021 = UNCERTAINTY_MEASURE_WITH_UNIT (LENGTH_MEASURE( 1.000000000000000082E-05 ), #13661, 'distance_accuracy_value', 'NONE');
#4022 = DIRECTION ( 'NONE',  ( 0.000000000000000000, 0.000000000000000000, 1.000000000000000000 ) ) ;
#4023 = CARTESIAN_POINT ( 'NONE',  ( 3.861362476283255685, 2.629030857715988656, -3.671615880910370500 ) ) ;
#4024 = EDGE_CURVE ( 'NONE', #13843, #2907, #5760, .T. ) ;
#4025 = EDGE_CURVE ( 'NONE', #9866, #5706, #6230, .T. ) ;
#4026 = CARTESIAN_POINT ( 'NONE',  ( 299.9999999999999432, -75.00000000000008527, 190.0000000000000000 ) ) ;
#4027 = ADVANCED_FACE ( 'NONE', ( #6465 ), #12027, .F. ) ;
#4028 = DIRECTION ( 'NONE',  ( -1.000000000000000000, 0.000000000000000000, 0.000000000000000000 ) ) ;
#4029 = EDGE_LOOP ( 'NONE', ( #2489, #1510, #14104, #7830 ) ) ;
#4030 = ORIENTED_EDGE ( 'NONE', *, *, #12798, .T. ) ;
#4031 = CARTESIAN_POINT ( 'NONE',  ( 303.3333333333333144, -14.99999999999999822, 219.8500000000001080 ) ) ;
#4032 = ORIENTED_EDGE ( 'NONE', *, *, #3891, .T. ) ;
#4033 = CARTESIAN_POINT ( 'NONE',  ( 53.33333333333330017, -20.00000000000000000, -222.5000000000000853 ) ) ;
#4034 = LINE ( 'NONE', #11573, #21 ) ;
#4035 = DIRECTION ( 'NONE',  ( -0.000000000000000000, -0.000000000000000000, -1.000000000000000000 ) ) ;
#4036 = VERTEX_POINT ( 'NONE', #7755 ) ;
#4037 = DIRECTION ( 'NONE',  ( 1.000000000000000000, 0.000000000000000000, 0.000000000000000000 ) ) ;
#4038 = CARTESIAN_POINT ( 'NONE',  ( 137.3500000000000227, -95.00000000000008527, -190.0000000000000000 ) ) ;
#4039 = DIRECTION ( 'NONE',  ( 6.123233995736766036E-17, 0.000000000000000000, 1.000000000000000000 ) ) ;
#4040 = CYLINDRICAL_SURFACE ( 'NONE', #5630, 2.500000000000000444 ) ;
#4041 = ADVANCED_BREP_SHAPE_REPRESENTATION ( '', ( #3882, #14039 ), #35 ) ;
#4042 = VERTEX_POINT ( 'NONE', #1144 ) ;
#4043 = ORIENTED_EDGE ( 'NONE', *, *, #1782, .F. ) ;
#4044 = FACE_OUTER_BOUND ( 'NONE', #12958, .T. ) ;
#4045 = PRODUCT_DEFINITION_SHAPE ( 'NONE', 'NONE',  #14346 ) ;
#4046 = ADVANCED_FACE ( 'NONE', ( #13337 ), #4367, .F. ) ;
#4047 = DIRECTION ( 'NONE',  ( -0.000000000000000000, -0.000000000000000000, -1.000000000000000000 ) ) ;
#4048 = ORIENTED_EDGE ( 'NONE', *, *, #6797, .T. ) ;
#4049 = CARTESIAN_POINT ( 'NONE',  ( 136.6666666666666288, -20.00000000000000000, 222.5000000000000853 ) ) ;
#4050 = DIRECTION ( 'NONE',  ( -0.000000000000000000, -0.000000000000000000, 1.000000000000000000 ) ) ;
#4051 = CARTESIAN_POINT ( 'NONE',  ( -4.211140560182196957, -2.431303136016552013, -3.745885042887436178 ) ) ;
#4052 = LINE ( 'NONE', #8401, #4402 ) ;
#4053 = DIRECTION ( 'NONE',  ( 1.000000000000000000, 0.000000000000000000, 0.000000000000000000 ) ) ;
#4054 = CLOSED_SHELL ( 'NONE', ( #11214, #4234, #8536, #7391, #7168, #7433, #11817, #3500, #9860, #8351, #4533, #13486, #5300, #8802, #1986, #6586, #10847, #7541, #13769, #1935, #7769, #6143, #5670, #3471, #3904, #4281, #10217, #9177, #383, #12001, #12659, #4881, #4852, #11918, #3251, #13760, #7110, #2696, #4147, #5633, #6429, #3042, #7531, #1983, #2691, #7940, #14138, #9609, #9070, #5079, #7651, #684, #8766, #6108, #5430, #7084, #4633, #8429, #13205, #11004, #7961, #13240, #86, #639, #2948, #12709, #6924, #1711, #12673, #1193, #8976, #6231, #8584, #8877, #11801, #1168, #4906, #3600, #1173, #3937, #7646, #10387, #3132, #1460, #12716, #3547, #9138, #446, #6223, #11729, #4518, #9240, #6831, #5775, #950, #244, #6754, #4563, #1478, #11450, #9151, #2590, #5673, #7898, #6844, #8788 ) ) ;
#4055 = CARTESIAN_POINT ( 'NONE',  ( 4.000000000000000000, 0.1981133338132474442, 2.382280164152719704E-17 ) ) ;
#4056 = EDGE_LOOP ( 'NONE', ( #1500, #8864, #14071, #10292 ) ) ;
#4057 = DIRECTION ( 'NONE',  ( 1.000000000000000000, 0.000000000000000000, 0.000000000000000000 ) ) ;
#4058 = VERTEX_POINT ( 'NONE', #12056 ) ;
#4059 = DIRECTION ( 'NONE',  ( -0.000000000000000000, -0.000000000000000000, 1.000000000000000000 ) ) ;
#4060 = LINE ( 'NONE', #7104, #12286 ) ;
#4061 = AXIS2_PLACEMENT_3D ( 'NONE', #11749, #628, #9503 ) ;
#4062 = VERTEX_POINT ( 'NONE', #2324 ) ;
#4063 = DIRECTION ( 'NONE',  ( 0.000000000000000000, 0.000000000000000000, -1.000000000000000000 ) ) ;
#4064 = ORIENTED_EDGE ( 'NONE', *, *, #3032, .T. ) ;
#4065 = DIRECTION ( 'NONE',  ( 0.000000000000000000, -0.000000000000000000, 1.000000000000000000 ) ) ;
#4066 = CARTESIAN_POINT ( 'NONE',  ( -4.000000000000000000, 0.1981133338132459731, 2.096406544454392723E-17 ) ) ;
#4067 = ORIENTED_EDGE ( 'NONE', *, *, #7259, .F. ) ;
#4068 = DIRECTION ( 'NONE',  ( -0.000000000000000000, -0.000000000000000000, -1.000000000000000000 ) ) ;
#4069 = EDGE_CURVE ( 'NONE', #6338, #12042, #10405, .T. ) ;
#4070 = PLANE ( 'NONE',  #4934 ) ;
#4071 = FILL_AREA_STYLE_COLOUR ( '', #3773 ) ;
#4072 = LINE ( 'NONE', #7481, #5345 ) ;
#4073 = CARTESIAN_POINT ( 'NONE',  ( 2.740000000000000213, 0.000000000000000000, 0.8509999999999999787 ) ) ;
#4074 = CIRCLE ( 'NONE', #2681, 2.649999999999985700 ) ;
#4075 = ORIENTED_EDGE ( 'NONE', *, *, #13590, .T. ) ;
#4076 = ORIENTED_EDGE ( 'NONE', *, *, #8041, .F. ) ;
#4077 = VERTEX_POINT ( 'NONE', #5382 ) ;
#4078 = ORIENTED_EDGE ( 'NONE', *, *, #3725, .F. ) ;
#4079 = DIRECTION ( 'NONE',  ( 1.000000000000000000, 0.000000000000000000, 0.000000000000000000 ) ) ;
#4080 = ORIENTED_EDGE ( 'NONE', *, *, #7815, .F. ) ;
#4081 = VERTEX_POINT ( 'NONE', #4291 ) ;
#4082 = CARTESIAN_POINT ( 'NONE',  ( 1.734723475976807094E-15, 4.618802153517012954, -0.4999999999999995559 ) ) ;
#4083 = ORIENTED_EDGE ( 'NONE', *, *, #6289, .T. ) ;
#4084 = CARTESIAN_POINT ( 'NONE',  ( 1.849560077140141257, -0.7556913915602415655, -0.5150000000000000133 ) ) ;
#4085 = AXIS2_PLACEMENT_3D ( 'NONE', #6459, #4065, #11759 ) ;
#4086 = LINE ( 'NONE', #1909, #11314 ) ;
#4087 = CARTESIAN_POINT ( 'NONE',  ( 2.449848172108560096, 3.432307619358740514, -3.503702292528905637 ) ) ;
#4088 = EDGE_CURVE ( 'NONE', #2372, #12902, #5657, .T. ) ;
#4089 = DIRECTION ( 'NONE',  ( -1.000000000000000000, -0.000000000000000000, -0.000000000000000000 ) ) ;
#4090 = CARTESIAN_POINT ( 'NONE',  ( -217.3499999999999375, -85.00000000000009948, 30.00000000000000000 ) ) ;
#4091 = AXIS2_PLACEMENT_3D ( 'NONE', #4770, #13339, #12186 ) ;
#4092 = ORIENTED_EDGE ( 'NONE', *, *, #12893, .F. ) ;
#4093 = AXIS2_PLACEMENT_3D ( 'NONE', #4929, #8102, #2893 ) ;
#4094 = EDGE_LOOP ( 'NONE', ( #10916, #7696, #8497, #8219 ) ) ;
#4095 = CONICAL_SURFACE ( 'NONE', #12890, 2.500000000000002220, 1.029744260000002631 ) ;
#4096 = EDGE_CURVE ( 'NONE', #486, #13503, #8993, .T. ) ;
#4097 = EDGE_CURVE ( 'NONE', #5874, #12188, #3490, .T. ) ;
#4099 = LINE ( 'NONE', #6128, #11881 ) ;
#4098 = AXIS2_PLACEMENT_3D ( 'NONE', #7985, #10255, #9161 ) ;
#4100 = ORIENTED_EDGE ( 'NONE', *, *, #2150, .F. ) ;
#4101 = DIRECTION ( 'NONE',  ( 0.000000000000000000, 0.000000000000000000, 1.000000000000000000 ) ) ;
#4102 = DIRECTION ( 'NONE',  ( -0.000000000000000000, -0.000000000000000000, -1.000000000000000000 ) ) ;
#4103 = LINE ( 'NONE', #7362, #8988 ) ;
#4104 = AXIS2_PLACEMENT_3D ( 'NONE', #2750, #2674, #12394 ) ;
#4105 = ORIENTED_EDGE ( 'NONE', *, *, #3548, .F. ) ;
#4106 = ADVANCED_FACE ( 'NONE', ( #5446, #3214 ), #14284, .F. ) ;
#4107 = VECTOR ( 'NONE', #7632, 1000.000000000000000 ) ;
#4108 = CARTESIAN_POINT ( 'NONE',  ( 305.0000000000000000, -56.99999999999997158, -180.0000000000000000 ) ) ;
#4109 = VECTOR ( 'NONE', #11777, 1000.000000000000000 ) ;
#4110 = CARTESIAN_POINT ( 'NONE',  ( 219.9999999999999716, -85.00000000000007105, 50.00000000000001421 ) ) ;
#4111 = CARTESIAN_POINT ( 'NONE',  ( 203.5000000000000000, -85.00000000000007105, 200.0000000000000000 ) ) ;
#4112 = CIRCLE ( 'NONE', #8508, 5.500000000000005329 ) ;
#4113 = LINE ( 'NONE', #12739, #11816 ) ;
#4114 = VERTEX_POINT ( 'NONE', #255 ) ;
#4115 = AXIS2_PLACEMENT_3D ( 'NONE', #8199, #4957, #10613 ) ;
#4116 = ORIENTED_EDGE ( 'NONE', *, *, #12433, .F. ) ;
#4117 = EDGE_CURVE ( 'NONE', #2687, #1127, #12482, .T. ) ;
#4118 = DIRECTION ( 'NONE',  ( -1.000000000000000000, -0.000000000000000000, -0.000000000000000000 ) ) ;
#4119 = VECTOR ( 'NONE', #10380, 1000.000000000000000 ) ;
#4120 = EDGE_CURVE ( 'NONE', #4659, #12287, #8779, .T. ) ;
#4121 = FACE_OUTER_BOUND ( 'NONE', #14146, .T. ) ;
#4122 = VECTOR ( 'NONE', #3994, 1000.000000000000000 ) ;
#4123 = CIRCLE ( 'NONE', #5473, 20.00000000000000000 ) ;
#4124 = ORIENTED_EDGE ( 'NONE', *, *, #3339, .F. ) ;
#4125 = CARTESIAN_POINT ( 'NONE',  ( 359.9999999999997726, 35.00000000000002842, 10.00000000000000000 ) ) ;
#4126 = EDGE_CURVE ( 'NONE', #13395, #8791, #10417, .T. ) ;
#4127 = PRODUCT_DEFINITION_CONTEXT ( 'detailed design', #9055, 'design' ) ;
#4128 = DIRECTION ( 'NONE',  ( -1.000000000000000000, 0.000000000000000000, 0.000000000000000000 ) ) ;
#4129 = CARTESIAN_POINT ( 'NONE',  ( 4.000000000000000000, -1.677850389431204459, -3.535268758346977513 ) ) ;
#4130 = CONICAL_SURFACE ( 'NONE', #2974, 2.500000000000002220, 1.029744260000002631 ) ;
#4131 = FACE_OUTER_BOUND ( 'NONE', #10936, .T. ) ;
#4132 = CONTEXT_DEPENDENT_SHAPE_REPRESENTATION ( #5757, #13878 ) ;
#4133 = ORIENTED_EDGE ( 'NONE', *, *, #747, .T. ) ;
#4134 = DIRECTION ( 'NONE',  ( 1.000000000000000000, 0.000000000000000000, 0.000000000000000000 ) ) ;
#4135 = ORIENTED_EDGE ( 'NONE', *, *, #7821, .T. ) ;
#4136 = DIRECTION ( 'NONE',  ( -0.000000000000000000, 0.000000000000000000, -1.000000000000000000 ) ) ;
#4137 = CARTESIAN_POINT ( 'NONE',  ( 259.0000000000000000, 8.660254037844390851, 199.9990000000000236 ) ) ;
#4138 = VERTEX_POINT ( 'NONE', #5799 ) ;
#4139 = DIRECTION ( 'NONE',  ( 1.007709689656716815E-16, 1.153406566473941260E-16, -1.000000000000000000 ) ) ;
#4140 = EDGE_LOOP ( 'NONE', ( #7914, #7190, #12359, #12426 ) ) ;
#4141 = CARTESIAN_POINT ( 'NONE',  ( 305.0000000000000000, -36.99999999999997868, -169.9999999999999716 ) ) ;
#4142 = DIRECTION ( 'NONE',  ( -1.000000000000000000, -0.000000000000000000, -0.000000000000000000 ) ) ;
#4143 = VERTEX_POINT ( 'NONE', #4722 ) ;
#4144 = PLANE ( 'NONE',  #11075 ) ;
#4145 = AXIS2_PLACEMENT_3D ( 'NONE', #13802, #8215, #12723 ) ;
#4146 = CYLINDRICAL_SURFACE ( 'NONE', #10866, 2.500000000000000444 ) ;
#4147 = ADVANCED_FACE ( 'NONE', ( #11526 ), #4936, .F. ) ;
#4148 = CARTESIAN_POINT ( 'NONE',  ( -4.204114297095464359, 1.660363174096617156, -3.602136431857887011 ) ) ;
#4149 = EDGE_LOOP ( 'NONE', ( #13454, #6233, #12323, #6418, #11456 ) ) ;
#4150 = VERTEX_POINT ( 'NONE', #8109 ) ;
#4151 = CARTESIAN_POINT ( 'NONE',  ( 0.000000000000000000, -225.0000000000000000, 0.000000000000000000 ) ) ;
#4152 = APPLICATION_CONTEXT ( 'automotive_design' ) ;
#4153 = ORIENTED_EDGE ( 'NONE', *, *, #1697, .F. ) ;
#4154 = DIRECTION ( 'NONE',  ( -1.000000000000000000, -0.000000000000000000, -0.000000000000000000 ) ) ;
#4155 = AXIS2_PLACEMENT_3D ( 'NONE', #13129, #8855, #14216 ) ;
#4156 = VERTEX_POINT ( 'NONE', #469 ) ;
#4157 = ORIENTED_EDGE ( 'NONE', *, *, #266, .F. ) ;
#4158 = CARTESIAN_POINT ( 'NONE',  ( -31.74999999999995737, 0.000000000000000000, 2.500000000000000444 ) ) ;
#4159 = ORIENTED_EDGE ( 'NONE', *, *, #12866, .F. ) ;
#4160 = DIRECTION ( 'NONE',  ( 0.000000000000000000, 0.000000000000000000, -1.000000000000000000 ) ) ;
#4161 = UNCERTAINTY_MEASURE_WITH_UNIT (LENGTH_MEASURE( 1.000000000000000082E-05 ), #7540, 'distance_accuracy_value', 'NONE');
#4162 = PLANE ( 'NONE',  #8969 ) ;
#4163 = CARTESIAN_POINT ( 'NONE',  ( -5.000000000000000888, 8.660254037844390851, 199.9990000000000236 ) ) ;
#4164 = DIRECTION ( 'NONE',  ( 1.000000000000000000, 0.000000000000000000, 0.000000000000000000 ) ) ;
#4165 = AXIS2_PLACEMENT_3D ( 'NONE', #9623, #674, #14036 ) ;
#4166 = DIRECTION ( 'NONE',  ( -0.000000000000000000, -0.000000000000000000, 1.000000000000000000 ) ) ;
#4167 = PRODUCT_DEFINITION_SHAPE ( 'NONE', 'NONE',  #14352 ) ;
#4168 = ORIENTED_EDGE ( 'NONE', *, *, #7745, .F. ) ;
#4169 = CIRCLE ( 'NONE', #5334, 2.649999999999985700 ) ;
#4170 = EDGE_LOOP ( 'NONE', ( #5892, #3998, #5411, #14236 ) ) ;
#4171 = EDGE_CURVE ( 'NONE', #4511, #10102, #11127, .T. ) ;
#4172 = DIRECTION ( 'NONE',  ( 0.000000000000000000, 0.000000000000000000, -1.000000000000000000 ) ) ;
#4173 = ADVANCED_FACE ( 'NONE', ( #5724 ), #11454, .F. ) ;
#4174 = VERTEX_POINT ( 'NONE', #8249 ) ;
#4175 = FACE_OUTER_BOUND ( 'NONE', #11152, .T. ) ;
#4176 = AXIS2_PLACEMENT_3D ( 'NONE', #7510, #6278, #10497 ) ;
#4177 = PLANE ( 'NONE',  #6085 ) ;
#4178 = DIRECTION ( 'NONE',  ( -0.000000000000000000, -0.000000000000000000, 1.000000000000000000 ) ) ;
#4179 = CIRCLE ( 'NONE', #11582, 2.649999999999985700 ) ;
#4180 = ORIENTED_EDGE ( 'NONE', *, *, #1697, .T. ) ;
#4181 = CIRCLE ( 'NONE', #432, 5.000000000000004441 ) ;
#4182 = VECTOR ( 'NONE', #3068, 1000.000000000000000 ) ;
#4183 = FACE_OUTER_BOUND ( 'NONE', #12513, .T. ) ;
#4184 = CARTESIAN_POINT ( 'NONE',  ( 0.000000000000000000, 2.350000000000000089, -0.5150000000000000133 ) ) ;
#4185 = DIRECTION ( 'NONE',  ( -1.000000000000000000, -6.123233995736766036E-17, -6.123233995736764803E-17 ) ) ;
#4186 = CARTESIAN_POINT ( 'NONE',  ( -3.999999999999999112, -2.309401076758512694, -3.504269196027871125 ) ) ;
#4187 = VERTEX_POINT ( 'NONE', #13620 ) ;
#4188 = VECTOR ( 'NONE', #12173, 1000.000000000000000 ) ;
#4189 = CIRCLE ( 'NONE', #11140, 2.500000000000002220 ) ;
#4190 = ORIENTED_EDGE ( 'NONE', *, *, #5427, .F. ) ;
#4191 = EDGE_CURVE ( 'NONE', #32, #10991, #1345, .T. ) ;
#4192 = DIRECTION ( 'NONE',  ( -1.000000000000000000, -0.000000000000000000, -0.000000000000000000 ) ) ;
#4193 = PRODUCT_RELATED_PRODUCT_CATEGORY ( 'part', '', ( #3346 ) ) ;
#4194 = PLANE ( 'NONE',  #5130 ) ;
#4195 = EDGE_LOOP ( 'NONE', ( #2759, #5420 ) ) ;
#4196 = LINE ( 'NONE', #6288, #3186 ) ;
#4197 = AXIS2_PLACEMENT_3D ( 'NONE', #826, #3113, #7376 ) ;
#4198 = CARTESIAN_POINT ( 'NONE',  ( 4.211140560182196957, -2.431303136016555122, -3.745885042887436622 ) ) ;
#4199 = ADVANCED_FACE ( 'NONE', ( #3695 ), #7031, .F. ) ;
#4200 = EDGE_CURVE ( 'NONE', #8612, #12266, #13479, .T. ) ;
#4201 = DIRECTION ( 'NONE',  ( -1.000000000000000000, 0.000000000000000000, 0.000000000000000000 ) ) ;
#4202 = EDGE_CURVE ( 'NONE', #8845, #7342, #171, .T. ) ;
#4203 = ADVANCED_FACE ( 'NONE', ( #3622 ), #10363, .T. ) ;
#4204 = AXIS2_PLACEMENT_3D ( 'NONE', #5982, #13801, #4833 ) ;
#4205 = VERTEX_POINT ( 'NONE', #1436 ) ;
#4206 = DIRECTION ( 'NONE',  ( 0.000000000000000000, 0.000000000000000000, 1.000000000000000000 ) ) ;
#4207 = VECTOR ( 'NONE', #10788, 1000.000000000000000 ) ;
#4208 = VERTEX_POINT ( 'NONE', #4863 ) ;
#4209 = CARTESIAN_POINT ( 'NONE',  ( 303.3333333333333144, -20.00000000000000000, 225.1500000000000625 ) ) ;
#4210 = CARTESIAN_POINT ( 'NONE',  ( -12.00000000000000000, 0.000000000000000000, 190.0000000000000000 ) ) ;
#4211 =( GEOMETRIC_REPRESENTATION_CONTEXT ( 3 ) GLOBAL_UNCERTAINTY_ASSIGNED_CONTEXT ( ( #990 ) ) GLOBAL_UNIT_ASSIGNED_CONTEXT ( ( #187, #6680, #11243 ) ) REPRESENTATION_CONTEXT ( 'NONE', 'WORKASPACE' ) );
#4212 = ORIENTED_EDGE ( 'NONE', *, *, #13180, .F. ) ;
#4213 = LINE ( 'NONE', #13252, #8272 ) ;
#4214 = ORIENTED_EDGE ( 'NONE', *, *, #3507, .T. ) ;
#4215 = CARTESIAN_POINT ( 'NONE',  ( 2.000000000000001776, 0.000000000000000000, 0.000000000000000000 ) ) ;
#4216 = CARTESIAN_POINT ( 'NONE',  ( 21.00000000000000355, 0.000000000000000000, 0.000000000000000000 ) ) ;
#4217 = ORIENTED_EDGE ( 'NONE', *, *, #6336, .F. ) ;
#4218 = LINE ( 'NONE', #12050, #11760 ) ;
#4219 = DIRECTION ( 'NONE',  ( 0.000000000000000000, 0.000000000000000000, 1.000000000000000000 ) ) ;
#4220 = SURFACE_STYLE_USAGE ( .BOTH. , #780 ) ;
#4221 = AXIS2_PLACEMENT_3D ( 'NONE', #1349, #5786, #13396 ) ;
#4222 =( NAMED_UNIT ( * ) PLANE_ANGLE_UNIT ( ) SI_UNIT ( $, .RADIAN. ) );
#4223 = CONTEXT_DEPENDENT_SHAPE_REPRESENTATION ( #3595, #983 ) ;
#4224 = DIRECTION ( 'NONE',  ( -0.000000000000000000, 0.000000000000000000, 1.000000000000000000 ) ) ;
#4225 =( GEOMETRIC_REPRESENTATION_CONTEXT ( 3 ) GLOBAL_UNCERTAINTY_ASSIGNED_CONTEXT ( ( #2175 ) ) GLOBAL_UNIT_ASSIGNED_CONTEXT ( ( #11453, #1645, #6084 ) ) REPRESENTATION_CONTEXT ( 'NONE', 'WORKASPACE' ) );
#4226 = ORIENTED_EDGE ( 'NONE', *, *, #693, .T. ) ;
#4227 = ORIENTED_EDGE ( 'NONE', *, *, #6491, .T. ) ;
#4228 = DIRECTION ( 'NONE',  ( 0.000000000000000000, -0.000000000000000000, 1.000000000000000000 ) ) ;
#4229 = SHAPE_REPRESENTATION ( 'stationary aligner', ( #14039 ), #35 ) ;
#4230 = VERTEX_POINT ( 'NONE', #12396 ) ;
#4231 = CARTESIAN_POINT ( 'NONE',  ( -4.024497503033714452, 2.323544716729487813, -3.572167766733750582 ) ) ;
#4232 = ORIENTED_EDGE ( 'NONE', *, *, #504, .T. ) ;
#4233 = VECTOR ( 'NONE', #3766, 1000.000000000000000 ) ;
#4234 = ADVANCED_FACE ( 'NONE', ( #9282 ), #6884, .F. ) ;
#4235 = EDGE_LOOP ( 'NONE', ( #9633, #6493 ) ) ;
#4236 = LINE ( 'NONE', #7196, #2008 ) ;
#4237 = EDGE_LOOP ( 'NONE', ( #6549, #792, #4293, #906 ) ) ;
#4238 = DIRECTION ( 'NONE',  ( 0.8949343913984144638, 0.4461977533474923430, 0.000000000000000000 ) ) ;
#4239 = AXIS2_PLACEMENT_3D ( 'NONE', #6212, #14037, #10645 ) ;
#4240 = CARTESIAN_POINT ( 'NONE',  ( 2.500000000000000000, 1.178949249685218525, 2.041999999999999371 ) ) ;
#4241 = DIRECTION ( 'NONE',  ( -1.000000000000000000, -0.000000000000000000, -0.000000000000000000 ) ) ;
#4242 = VECTOR ( 'NONE', #7037, 1000.000000000000000 ) ;
#4243 = DIRECTION ( 'NONE',  ( 1.000000000000000000, 0.000000000000000000, 0.000000000000000000 ) ) ;
#4244 = CARTESIAN_POINT ( 'NONE',  ( 210.0000000000000000, -85.00000000000007105, 170.0000000000000000 ) ) ;
#4246 = AXIS2_PLACEMENT_3D ( 'NONE', #779, #1890, #1816 ) ;
#4245 = AXIS2_PLACEMENT_3D ( 'NONE', #10708, #5203, #10555 ) ;
#4247 = ORIENTED_EDGE ( 'NONE', *, *, #9968, .F. ) ;
#4248 = EDGE_LOOP ( 'NONE', ( #3513, #677, #474, #11762 ) ) ;
#4249 = PRODUCT_DEFINITION_FORMATION_WITH_SPECIFIED_SOURCE ( 'ANY', '', #173, .NOT_KNOWN. ) ;
#4250 = LINE ( 'NONE', #8665, #1201 ) ;
#4251 = EDGE_LOOP ( 'NONE', ( #6690, #2662 ) ) ;
#4252 = CARTESIAN_POINT ( 'NONE',  ( 2.500000000000000000, 1.178949249685217415, 2.041999999999998483 ) ) ;
#4253 = DIRECTION ( 'NONE',  ( -0.000000000000000000, 0.000000000000000000, -1.000000000000000000 ) ) ;
#4254 = VECTOR ( 'NONE', #8256, 1000.000000000000000 ) ;
#4255 = PLANE ( 'NONE',  #12459 ) ;
#4256 = VERTEX_POINT ( 'NONE', #8178 ) ;
#4257 = FACE_BOUND ( 'NONE', #9141, .T. ) ;
#4258 = ADVANCED_FACE ( 'NONE', ( #7094 ), #1241, .F. ) ;
#4259 = DIRECTION ( 'NONE',  ( 1.007709689656716815E-16, 1.000000000000000000, 3.606821995490527259E-15 ) ) ;
#4260 = DIRECTION ( 'NONE',  ( 1.000000000000000000, 0.000000000000000000, 6.123233995736766036E-17 ) ) ;
#4261 = DIRECTION ( 'NONE',  ( 1.000000000000000000, 0.000000000000000000, -0.000000000000000000 ) ) ;
#4262 = ORIENTED_EDGE ( 'NONE', *, *, #13239, .F. ) ;
#4263 = ORIENTED_EDGE ( 'NONE', *, *, #7726, .T. ) ;
#4264 = CARTESIAN_POINT ( 'NONE',  ( 2.500000000000000000, -1.178949249685213863, 2.042000000000002924 ) ) ;
#4265 = LINE ( 'NONE', #13036, #11147 ) ;
#4266 = VERTEX_POINT ( 'NONE', #8467 ) ;
#4267 = FACE_OUTER_BOUND ( 'NONE', #3076, .T. ) ;
#4268 = EDGE_CURVE ( 'NONE', #9383, #1332, #9944, .T. ) ;
#4269 = PRODUCT_RELATED_PRODUCT_CATEGORY ( 'part', '', ( #10165 ) ) ;
#4270 = CARTESIAN_POINT ( 'NONE',  ( 2.000000000000008882, 3.464101615137749945, 0.000000000000000000 ) ) ;
#4271 = CARTESIAN_POINT ( 'NONE',  ( 303.3333333333333144, -30.00000000000000355, 222.5000000000000853 ) ) ;
#4272 = ORIENTED_EDGE ( 'NONE', *, *, #344, .F. ) ;
#4273 = DIRECTION ( 'NONE',  ( -0.000000000000000000, 1.000000000000000000, -0.000000000000000000 ) ) ;
#4274 = ORIENTED_EDGE ( 'NONE', *, *, #13487, .F. ) ;
#4275 = DIRECTION ( 'NONE',  ( -0.000000000000000000, 1.000000000000000000, -0.000000000000000000 ) ) ;
#4276 = FACE_OUTER_BOUND ( 'NONE', #11088, .T. ) ;
#4277 = EDGE_CURVE ( 'NONE', #5030, #11926, #2523, .T. ) ;
#4278 = EDGE_CURVE ( 'NONE', #5507, #10102, #8519, .T. ) ;
#4279 =( REPRESENTATION_RELATIONSHIP ('NONE','NONE', #11251, #10713 ) REPRESENTATION_RELATIONSHIP_WITH_TRANSFORMATION ( #11599 )SHAPE_REPRESENTATION_RELATIONSHIP( ) );
#4280 = VERTEX_POINT ( 'NONE', #1721 ) ;
#4281 = ADVANCED_FACE ( 'NONE', ( #624 ), #10163, .F. ) ;
#4282 = ORIENTED_EDGE ( 'NONE', *, *, #371, .F. ) ;
#4283 = DIRECTION ( 'NONE',  ( 1.000000000000000000, 0.000000000000000000, 0.000000000000000000 ) ) ;
#4284 = PRODUCT_DEFINITION_SHAPE ( 'NONE', 'NONE',  #14374 ) ;
#4285 = DIRECTION ( 'NONE',  ( 0.000000000000000000, 0.000000000000000000, 1.000000000000000000 ) ) ;
#4286 = VECTOR ( 'NONE', #10463, 1000.000000000000000 ) ;
#4287 = EDGE_LOOP ( 'NONE', ( #11625, #4346, #13827, #9504 ) ) ;
#4288 = DIRECTION ( 'NONE',  ( -0.000000000000000000, 1.000000000000000000, -0.000000000000000000 ) ) ;
#4289 = DIRECTION ( 'NONE',  ( 0.000000000000000000, -0.000000000000000000, -1.000000000000000000 ) ) ;
#4290 = DIRECTION ( 'NONE',  ( 0.000000000000000000, 0.000000000000000000, -1.000000000000000000 ) ) ;
#4291 = CARTESIAN_POINT ( 'NONE',  ( 444.9999999999999432, -8.660254037844389075, 200.0000000000000000 ) ) ;
#4292 = DIRECTION ( 'NONE',  ( 0.000000000000000000, 0.000000000000000000, -1.000000000000000000 ) ) ;
#4293 = ORIENTED_EDGE ( 'NONE', *, *, #2511, .T. ) ;
#4294 = ORIENTED_EDGE ( 'NONE', *, *, #3659, .T. ) ;
#4295 = CARTESIAN_POINT ( 'NONE',  ( -140.0000000000000000, -75.00000000000008527, 40.00000000000000000 ) ) ;
#4296 = AXIS2_PLACEMENT_3D ( 'NONE', #9579, #7035, #11458 ) ;
#4297 = TOROIDAL_SURFACE ( 'NONE', #10786, 4.000000000000000000, 0.2500000000000000000 ) ;
#4298 = ORIENTED_EDGE ( 'NONE', *, *, #3235, .T. ) ;
#4299 = DIRECTION ( 'NONE',  ( -0.000000000000000000, -0.000000000000000000, -1.000000000000000000 ) ) ;
#4300 = EDGE_LOOP ( 'NONE', ( #9971, #55, #12916, #12028, #5157 ) ) ;
#4301 = EDGE_CURVE ( 'NONE', #13571, #3125, #2752, .T. ) ;
#4302 = VERTEX_POINT ( 'NONE', #10876 ) ;
#4303 = CARTESIAN_POINT ( 'NONE',  ( 299.9999999999999432, -95.00000000000008527, 190.0000000000000000 ) ) ;
#4304 = ORIENTED_EDGE ( 'NONE', *, *, #12094, .F. ) ;
#4305 = DIRECTION ( 'NONE',  ( -0.000000000000000000, 1.000000000000000000, -0.000000000000000000 ) ) ;
#4306 = FACE_OUTER_BOUND ( 'NONE', #3081, .T. ) ;
#4307 = CARTESIAN_POINT ( 'NONE',  ( 2.500000000000000000, -1.178949249685218748, -2.041999999999998039 ) ) ;
#4308 = CYLINDRICAL_SURFACE ( 'NONE', #8544, 10.00000000000000888 ) ;
#4309 = AXIS2_PLACEMENT_3D ( 'NONE', #9075, #1373, #3568 ) ;
#4310 = FACE_OUTER_BOUND ( 'NONE', #1158, .T. ) ;
#4311 = FACE_OUTER_BOUND ( 'NONE', #3794, .T. ) ;
#4312 = ORIENTED_EDGE ( 'NONE', *, *, #5068, .F. ) ;
#4313 = ORIENTED_EDGE ( 'NONE', *, *, #2959, .T. ) ;
#4314 = CARTESIAN_POINT ( 'NONE',  ( 2.500000000000000000, 0.000000000000000000, 0.000000000000000000 ) ) ;
#4315 = VECTOR ( 'NONE', #11236, 1000.000000000000000 ) ;
#4316 = VERTEX_POINT ( 'NONE', #14120 ) ;
#4317 = PLANE ( 'NONE',  #10343 ) ;
#4318 = FACE_OUTER_BOUND ( 'NONE', #6945, .T. ) ;
#4319 = FACE_BOUND ( 'NONE', #1172, .T. ) ;
#4320 = ORIENTED_EDGE ( 'NONE', *, *, #9344, .F. ) ;
#4321 = VECTOR ( 'NONE', #8310, 1000.000000000000000 ) ;
#4322 = DIRECTION ( 'NONE',  ( -1.000000000000000000, -0.000000000000000000, -0.000000000000000000 ) ) ;
#4323 = CIRCLE ( 'NONE', #8007, 2.500000000000002220 ) ;
#4324 = CARTESIAN_POINT ( 'NONE',  ( 136.6666666666666288, -20.00000000000000000, 225.1500000000000625 ) ) ;
#4325 = DIRECTION ( 'NONE',  ( 6.123233995736766036E-17, 0.000000000000000000, -1.000000000000000000 ) ) ;
#4326 = CARTESIAN_POINT ( 'NONE',  ( 470.0000000000000000, -20.00000000000000000, -250.0000000000000000 ) ) ;
#4327 = EDGE_CURVE ( 'NONE', #2687, #2542, #404, .T. ) ;
#4328 = CIRCLE ( 'NONE', #4098, 2.100000000000000089 ) ;
#4329 = EDGE_LOOP ( 'NONE', ( #9699, #789, #2969, #7377 ) ) ;
#4330 = EDGE_LOOP ( 'NONE', ( #7525, #6508, #5557 ) ) ;
#4331 = DIRECTION ( 'NONE',  ( 1.000000000000000000, 0.000000000000000000, 0.000000000000000000 ) ) ;
#4332 = CIRCLE ( 'NONE', #6180, 2.500000000000002220 ) ;
#4333 = CARTESIAN_POINT ( 'NONE',  ( -996.9834933385058093, 0.000000000000000000, 0.000000000000000000 ) ) ;
#4334 = VECTOR ( 'NONE', #3893, 1000.000000000000000 ) ;
#4335 = VECTOR ( 'NONE', #6103, 1000.000000000000000 ) ;
#4336 = ORIENTED_EDGE ( 'NONE', *, *, #12038, .T. ) ;
#4337 = DIRECTION ( 'NONE',  ( 0.000000000000000000, 0.000000000000000000, 1.000000000000000000 ) ) ;
#4338 = VECTOR ( 'NONE', #1748, 1000.000000000000000 ) ;
#4339 = CIRCLE ( 'NONE', #6872, 5.500000000000005329 ) ;
#4340 = LINE ( 'NONE', #8761, #12199 ) ;
#4341 = PLANE ( 'NONE',  #5551 ) ;
#4342 = CARTESIAN_POINT ( 'NONE',  ( 439.9999999999999432, 0.000000000000000000, -188.0000000000000000 ) ) ;
#4343 = CIRCLE ( 'NONE', #10844, 2.649999999999985700 ) ;
#4344 =( REPRESENTATION_RELATIONSHIP ('NONE','NONE', #11251, #13104 ) REPRESENTATION_RELATIONSHIP_WITH_TRANSFORMATION ( #2108 )SHAPE_REPRESENTATION_RELATIONSHIP( ) );
#4345 =( GEOMETRIC_REPRESENTATION_CONTEXT ( 3 ) GLOBAL_UNCERTAINTY_ASSIGNED_CONTEXT ( ( #3009 ) ) GLOBAL_UNIT_ASSIGNED_CONTEXT ( ( #1234, #13559, #7768 ) ) REPRESENTATION_CONTEXT ( 'NONE', 'WORKASPACE' ) );
#4346 = ORIENTED_EDGE ( 'NONE', *, *, #7170, .T. ) ;
#4347 = VECTOR ( 'NONE', #14132, 1000.000000000000114 ) ;
#4348 = DIRECTION ( 'NONE',  ( -1.000000000000000000, -0.000000000000000000, -0.000000000000000000 ) ) ;
#4349 = AXIS2_PLACEMENT_3D ( 'NONE', #12047, #8919, #2100 ) ;
#4350 = ORIENTED_EDGE ( 'NONE', *, *, #8619, .F. ) ;
#4351 = FACE_OUTER_BOUND ( 'NONE', #12084, .T. ) ;
#4352 = DIRECTION ( 'NONE',  ( 0.000000000000000000, -1.000000000000000000, 0.000000000000000000 ) ) ;
#4353 = EDGE_CURVE ( 'NONE', #930, #4652, #2975, .T. ) ;
#4354 = ADVANCED_FACE ( 'NONE', ( #2010 ), #13837, .F. ) ;
#4355 = AXIS2_PLACEMENT_3D ( 'NONE', #3141, #5522, #4369 ) ;
#4356 = VERTEX_POINT ( 'NONE', #10661 ) ;
#4357 = ORIENTED_EDGE ( 'NONE', *, *, #10565, .T. ) ;
#4358 = CARTESIAN_POINT ( 'NONE',  ( 4.999999999999999112, 8.660254037844390851, -210.0000000000000000 ) ) ;
#4359 = UNCERTAINTY_MEASURE_WITH_UNIT (LENGTH_MEASURE( 1.000000000000000082E-05 ), #7754, 'distance_accuracy_value', 'NONE');
#4360 = AXIS2_PLACEMENT_3D ( 'NONE', #3553, #12391, #1063 ) ;
#4361 = DIRECTION ( 'NONE',  ( 0.000000000000000000, 0.000000000000000000, -1.000000000000000000 ) ) ;
#4362 = CARTESIAN_POINT ( 'NONE',  ( 7.345657149124338758, 1.312408941150044583, 0.000000000000000000 ) ) ;
#4363 = VECTOR ( 'NONE', #8597, 1000.000000000000000 ) ;
#4364 = FACE_OUTER_BOUND ( 'NONE', #10291, .T. ) ;
#4365 = DIRECTION ( 'NONE',  ( -1.000000000000000000, -0.000000000000000000, -0.000000000000000000 ) ) ;
#4366 = LINE ( 'NONE', #7753, #582 ) ;
#4367 = PLANE ( 'NONE',  #11108 ) ;
#4368 = EDGE_CURVE ( 'NONE', #9829, #50, #7384, .T. ) ;
#4369 = DIRECTION ( 'NONE',  ( 1.000000000000000000, 0.000000000000000000, 0.000000000000000000 ) ) ;
#4370 = EDGE_LOOP ( 'NONE', ( #6334, #6427, #330 ) ) ;
#4371 = ORIENTED_EDGE ( 'NONE', *, *, #4368, .F. ) ;
#4372 = PLANE ( 'NONE',  #9620 ) ;
#4373 = ORIENTED_EDGE ( 'NONE', *, *, #12655, .T. ) ;
#4374 = CARTESIAN_POINT ( 'NONE',  ( 136.6666666666666288, -20.00000000000000000, -222.5000000000000853 ) ) ;
#4375 = EDGE_CURVE ( 'NONE', #10192, #13567, #7309, .T. ) ;
#4376 = ORIENTED_EDGE ( 'NONE', *, *, #6491, .F. ) ;
#4377 = VECTOR ( 'NONE', #8289, 1000.000000000000000 ) ;
#4378 = ORIENTED_EDGE ( 'NONE', *, *, #11183, .T. ) ;
#4379 = DIRECTION ( 'NONE',  ( -1.000000000000000000, 0.000000000000000000, 0.000000000000000000 ) ) ;
#4380 = ORIENTED_EDGE ( 'NONE', *, *, #9949, .F. ) ;
#4381 = CARTESIAN_POINT ( 'NONE',  ( 137.6499999999999488, -36.99999999999997868, 0.000000000000000000 ) ) ;
#4382 = PRODUCT ( 'side rail', 'side rail', '', ( #4884 ) ) ;
#4383 = CARTESIAN_POINT ( 'NONE',  ( 136.6666666666666288, -14.99999999999999822, 222.5000000000000853 ) ) ;
#4384 = CARTESIAN_POINT ( 'NONE',  ( 302.6499999999999204, -75.00000000000008527, 190.0000000000000000 ) ) ;
#4385 = CARTESIAN_POINT ( 'NONE',  ( 4.999999999999999112, -8.660254037844389075, 200.0000000000000000 ) ) ;
#4386 = DIRECTION ( 'NONE',  ( 1.000000000000000000, 0.000000000000000000, 0.000000000000000000 ) ) ;
#4387 = EDGE_CURVE ( 'NONE', #7915, #7212, #3457, .T. ) ;
#4388 = EDGE_CURVE ( 'NONE', #8912, #5974, #689, .T. ) ;
#4389 = CARTESIAN_POINT ( 'NONE',  ( 197.5000000000000000, -90.00000000000007105, 55.00000000000001421 ) ) ;
#4390 = ORIENTED_EDGE ( 'NONE', *, *, #9123, .T. ) ;
#4391 = EDGE_CURVE ( 'NONE', #2488, #2710, #7388, .T. ) ;
#4392 = ADVANCED_FACE ( 'NONE', ( #5154, #4131 ), #6372, .F. ) ;
#4393 = AXIS2_PLACEMENT_3D ( 'NONE', #8783, #6746, #11176 ) ;
#4394 = ORIENTED_EDGE ( 'NONE', *, *, #7895, .F. ) ;
#4395 = EDGE_CURVE ( 'NONE', #12266, #722, #5362, .T. ) ;
#4396 = DIRECTION ( 'NONE',  ( 0.000000000000000000, 0.4999999999999990008, -0.8660254037844391517 ) ) ;
#4397 = ORIENTED_EDGE ( 'NONE', *, *, #5628, .T. ) ;
#4398 = CARTESIAN_POINT ( 'NONE',  ( -4.000000000000000000, -2.309401076758515803, -0.4999999999999995559 ) ) ;
#4399 = DIRECTION ( 'NONE',  ( 0.000000000000000000, -1.000000000000000000, -3.702006032529638986E-15 ) ) ;
#4400 = FILL_AREA_STYLE ('',( #4682 ) ) ;
#4401 = ORIENTED_EDGE ( 'NONE', *, *, #10040, .F. ) ;
#4402 = VECTOR ( 'NONE', #978, 1000.000000000000000 ) ;
#4403 = DIRECTION ( 'NONE',  ( -0.000000000000000000, -0.000000000000000000, 1.000000000000000000 ) ) ;
#4404 = AXIS2_PLACEMENT_3D ( 'NONE', #1306, #4665, #11405 ) ;
#4405 = CARTESIAN_POINT ( 'NONE',  ( 319.9999999999999432, -20.00000000000000000, 19.99999999999998934 ) ) ;
#4406 = DIRECTION ( 'NONE',  ( -0.000000000000000000, 1.000000000000000000, -0.000000000000000000 ) ) ;
#4407 = DIRECTION ( 'NONE',  ( -0.000000000000000000, 1.000000000000000000, -0.000000000000000000 ) ) ;
#4408 = ORIENTED_EDGE ( 'NONE', *, *, #825, .T. ) ;
#4409 = CIRCLE ( 'NONE', #429, 13.29999999999999893 ) ;
#4410 = PLANE ( 'NONE',  #220 ) ;
#4411 = VECTOR ( 'NONE', #11096, 1000.000000000000000 ) ;
#4412 = CARTESIAN_POINT ( 'NONE',  ( 0.2500000000000002220, 5.204748896376250699E-16, -4.250000000000000000 ) ) ;
#4413 =( GEOMETRIC_REPRESENTATION_CONTEXT ( 3 ) GLOBAL_UNCERTAINTY_ASSIGNED_CONTEXT ( ( #8507 ) ) GLOBAL_UNIT_ASSIGNED_CONTEXT ( ( #6830, #9894, #1236 ) ) REPRESENTATION_CONTEXT ( 'NONE', 'WORKASPACE' ) );
#4414 = EDGE_CURVE ( 'NONE', #11304, #3344, #761, .T. ) ;
#4415 = ORIENTED_EDGE ( 'NONE', *, *, #7815, .T. ) ;
#4416 = CARTESIAN_POINT ( 'NONE',  ( 1.144235203016666258, 3.958177651039090250, -0.09382832055445661235 ) ) ;
#4417 = DIRECTION ( 'NONE',  ( 0.000000000000000000, -0.000000000000000000, 1.000000000000000000 ) ) ;
#4418 = FACE_OUTER_BOUND ( 'NONE', #3427, .T. ) ;
#4419 = DIRECTION ( 'NONE',  ( 0.000000000000000000, 0.000000000000000000, 1.000000000000000000 ) ) ;
#4420 = AXIS2_PLACEMENT_3D ( 'NONE', #5290, #4192, #9630 ) ;
#4421 = AXIS2_PLACEMENT_3D ( 'NONE', #389, #5866, #4859 ) ;
#4422 = ORIENTED_EDGE ( 'NONE', *, *, #3830, .F. ) ;
#4423 = DIRECTION ( 'NONE',  ( 1.000000000000000000, 0.000000000000000000, 0.000000000000000000 ) ) ;
#4424 = EDGE_LOOP ( 'NONE', ( #9455, #9629, #11414, #4001, #11661 ) ) ;
#4425 = CARTESIAN_POINT ( 'NONE',  ( -4.000000000000000000, -1.942223658245633811, -0.3516579909967644246 ) ) ;
#4426 = EDGE_CURVE ( 'NONE', #9773, #5388, #11893, .T. ) ;
#4427 = VECTOR ( 'NONE', #3670, 1000.000000000000000 ) ;
#4428 = ORIENTED_EDGE ( 'NONE', *, *, #9314, .T. ) ;
#4429 = VERTEX_POINT ( 'NONE', #835 ) ;
#4430 = DIRECTION ( 'NONE',  ( 0.000000000000000000, -1.224646799147352468E-16, 1.000000000000000000 ) ) ;
#4431 = CARTESIAN_POINT ( 'NONE',  ( -4.235886605889389145, -2.417314728048544303, -3.751161874094020909 ) ) ;
#4432 = DIRECTION ( 'NONE',  ( 1.000000000000000000, 0.000000000000000000, 0.000000000000000000 ) ) ;
#4433 = CIRCLE ( 'NONE', #11148, 0.2000000000000022593 ) ;
#4434 = FACE_OUTER_BOUND ( 'NONE', #3780, .T. ) ;
#4435 = CARTESIAN_POINT ( 'NONE',  ( 134.5000000000000000, -75.00000000000008527, 190.0000000000000000 ) ) ;
#4436 = DIRECTION ( 'NONE',  ( 1.000000000000000000, 0.000000000000000000, 0.000000000000000000 ) ) ;
#4437 =( NAMED_UNIT ( * ) SI_UNIT ( $, .STERADIAN. ) SOLID_ANGLE_UNIT ( ) );
#4438 = DIRECTION ( 'NONE',  ( 0.000000000000000000, -0.5000000000000012212, -0.8660254037844380415 ) ) ;
#4439 = ADVANCED_FACE ( 'NONE', ( #12752, #7243, #6155, #11670, #622, #5083, #3982 ), #5297, .F. ) ;
#4440 = CARTESIAN_POINT ( 'NONE',  ( -4.000000000000000000, 0.8576368993457507139, -3.433240632782198709 ) ) ;
#4441 = ORIENTED_EDGE ( 'NONE', *, *, #11212, .F. ) ;
#4442 = ORIENTED_EDGE ( 'NONE', *, *, #12814, .F. ) ;
#4443 = CARTESIAN_POINT ( 'NONE',  ( 219.9999999999999716, -20.00000000000000000, 219.8500000000001080 ) ) ;
#4444 = ORIENTED_EDGE ( 'NONE', *, *, #164, .F. ) ;
#4445 = CIRCLE ( 'NONE', #8096, 5.000000000000004441 ) ;
#4446 = DIRECTION ( 'NONE',  ( -0.000000000000000000, -0.000000000000000000, -1.000000000000000000 ) ) ;
#4447 = ORIENTED_EDGE ( 'NONE', *, *, #9707, .T. ) ;
#4448 = LINE ( 'NONE', #8868, #13591 ) ;
#4449 = ORIENTED_EDGE ( 'NONE', *, *, #1489, .F. ) ;
#4450 = DIRECTION ( 'NONE',  ( -0.000000000000000000, -0.000000000000000000, 1.000000000000000000 ) ) ;
#4451 = LINE ( 'NONE', #2408, #11517 ) ;
#4452 = DIRECTION ( 'NONE',  ( 0.000000000000000000, -1.000000000000000000, 0.000000000000000000 ) ) ;
#4453 = DIRECTION ( 'NONE',  ( 1.000000000000000000, 0.000000000000000000, 0.000000000000000000 ) ) ;
#4454 = PRESENTATION_STYLE_ASSIGNMENT (( #13967 ) ) ;
#4455 = CARTESIAN_POINT ( 'NONE',  ( 2.500000000000000000, -1.178949249685214307, 2.042000000000001592 ) ) ;
#4456 = EDGE_CURVE ( 'NONE', #13972, #10462, #2895, .T. ) ;
#4457 = EDGE_CURVE ( 'NONE', #2121, #5322, #10649, .T. ) ;
#4458 = CARTESIAN_POINT ( 'NONE',  ( 119.9999999999999147, -25.00000000000000000, -169.9999999999999716 ) ) ;
#4459 = ORIENTED_EDGE ( 'NONE', *, *, #10381, .T. ) ;
#4460 = ORIENTED_EDGE ( 'NONE', *, *, #9569, .F. ) ;
#4461 = CIRCLE ( 'NONE', #8135, 13.50000000000000533 ) ;
#4462 = LINE ( 'NONE', #3240, #8398 ) ;
#4463 = AXIS2_PLACEMENT_3D ( 'NONE', #2737, #1482, #7152 ) ;
#4464 = MECHANICAL_DESIGN_GEOMETRIC_PRESENTATION_REPRESENTATION (  '', ( #8860 ), #462 ) ;
#4465 = ORIENTED_EDGE ( 'NONE', *, *, #11034, .T. ) ;
#4466 = LINE ( 'NONE', #12363, #7791 ) ;
#4467 = VECTOR ( 'NONE', #6821, 1000.000000000000000 ) ;
#4468 = LINE ( 'NONE', #7853, #2244 ) ;
#4469 = EDGE_CURVE ( 'NONE', #298, #9222, #4052, .T. ) ;
#4470 = EDGE_CURVE ( 'NONE', #6109, #9773, #6727, .T. ) ;
#4471 = DIRECTION ( 'NONE',  ( -1.000000000000000000, 0.000000000000000000, 0.000000000000000000 ) ) ;
#4472 = ORIENTED_EDGE ( 'NONE', *, *, #11702, .F. ) ;
#4473 = ADVANCED_FACE ( 'NONE', ( #4418 ), #14195, .T. ) ;
#4474 = AXIS2_PLACEMENT_3D ( 'NONE', #11432, #6720, #2369 ) ;
#4475 = FACE_BOUND ( 'NONE', #6477, .T. ) ;
#4476 = FACE_OUTER_BOUND ( 'NONE', #3861, .T. ) ;
#4477 = PRODUCT_DEFINITION_FORMATION_WITH_SPECIFIED_SOURCE ( 'ANY', '', #10055, .NOT_KNOWN. ) ;
#4478 = CARTESIAN_POINT ( 'NONE',  ( -30.00000000000002842, -25.00000000000000000, -190.0000000000000000 ) ) ;
#4479 =( GEOMETRIC_REPRESENTATION_CONTEXT ( 3 ) GLOBAL_UNCERTAINTY_ASSIGNED_CONTEXT ( ( #9868 ) ) GLOBAL_UNIT_ASSIGNED_CONTEXT ( ( #5519, #4648, #4437 ) ) REPRESENTATION_CONTEXT ( 'NONE', 'WORKASPACE' ) );
#4480 = CARTESIAN_POINT ( 'NONE',  ( -4.000000000000000000, -2.309401076758512694, -3.433295621305382461 ) ) ;
#4481 = VECTOR ( 'NONE', #2835, 1000.000000000000000 ) ;
#4482 = ORIENTED_EDGE ( 'NONE', *, *, #12474, .F. ) ;
#4483 = DIRECTION ( 'NONE',  ( -1.000000000000000000, 0.000000000000000000, -0.000000000000000000 ) ) ;
#4484 = VECTOR ( 'NONE', #10993, 1000.000000000000000 ) ;
#4485 = CARTESIAN_POINT ( 'NONE',  ( 145.5000000000000284, -75.00000000000008527, -190.0000000000000000 ) ) ;
#4486 = DIRECTION ( 'NONE',  ( 0.000000000000000000, 0.000000000000000000, 1.000000000000000000 ) ) ;
#4487 = ORIENTED_EDGE ( 'NONE', *, *, #12241, .T. ) ;
#4488 = CARTESIAN_POINT ( 'NONE',  ( 134.9999999999999716, 45.00000000000001421, 0.000000000000000000 ) ) ;
#4489 = FACE_OUTER_BOUND ( 'NONE', #9216, .T. ) ;
#4490 = LINE ( 'NONE', #5641, #14115 ) ;
#4491 = DIRECTION ( 'NONE',  ( 0.000000000000000000, 0.000000000000000000, 1.000000000000000000 ) ) ;
#4492 = EDGE_CURVE ( 'NONE', #12063, #9564, #13320, .T. ) ;
#4493 = VERTEX_POINT ( 'NONE', #7801 ) ;
#4494 = FACE_OUTER_BOUND ( 'NONE', #8698, .T. ) ;
#4495 = PRODUCT ( 'actuator', 'actuator', '', ( #4956 ) ) ;
#4496 = ORIENTED_EDGE ( 'NONE', *, *, #7304, .F. ) ;
#4497 = CARTESIAN_POINT ( 'NONE',  ( 1.257172072275274388, -3.892973519170983110, -3.433252694550781303 ) ) ;
#4498 = VERTEX_POINT ( 'NONE', #3469 ) ;
#4499 = ORIENTED_EDGE ( 'NONE', *, *, #10635, .F. ) ;
#4500 = CARTESIAN_POINT ( 'NONE',  ( 1.424271237134740131, 0.000000000000000000, 4.556291390728477886 ) ) ;
#4501 = PLANE ( 'NONE',  #9172 ) ;
#4502 = LINE ( 'NONE', #12180, #849 ) ;
#4503 = CARTESIAN_POINT ( 'NONE',  ( -299.9999999999999432, -75.00000000000008527, 328.4978484569338661 ) ) ;
#4504 = CARTESIAN_POINT ( 'NONE',  ( -299.9999999999999432, -75.00000000000008527, 10.00000000000000178 ) ) ;
#4505 = DIRECTION ( 'NONE',  ( -1.000000000000000000, 0.000000000000000000, 0.000000000000000000 ) ) ;
#4506 = CARTESIAN_POINT ( 'NONE',  ( -5.000000000000000888, -8.660254037844389075, 210.0000000000000000 ) ) ;
#4507 = ITEM_DEFINED_TRANSFORMATION ( 'NONE', 'NONE', #12780,  #14039 ) ;
#4508 = CYLINDRICAL_SURFACE ( 'NONE', #2705, 2.649999999999985700 ) ;
#4509 = ORIENTED_EDGE ( 'NONE', *, *, #3862, .F. ) ;
#4510 = ADVANCED_FACE ( 'NONE', ( #8835 ), #5428, .F. ) ;
#4511 = VERTEX_POINT ( 'NONE', #4270 ) ;
#4512 = CARTESIAN_POINT ( 'NONE',  ( 4.999999999999999112, 8.660254037844390851, 205.0000000000000284 ) ) ;
#4513 = ORIENTED_EDGE ( 'NONE', *, *, #11633, .T. ) ;
#4514 = CARTESIAN_POINT ( 'NONE',  ( -4.211140560182196957, 2.431303136016537803, -3.745885042887433514 ) ) ;
#4515 = ORIENTED_EDGE ( 'NONE', *, *, #8041, .T. ) ;
#4516 = FACE_BOUND ( 'NONE', #1505, .T. ) ;
#4517 = ORIENTED_EDGE ( 'NONE', *, *, #3753, .T. ) ;
#4518 = ADVANCED_FACE ( 'NONE', ( #6658, #1199 ), #4341, .F. ) ;
#4519 = DIRECTION ( 'NONE',  ( 1.000000000000000000, 0.000000000000000000, -0.000000000000000000 ) ) ;
#4520 = LINE ( 'NONE', #13352, #12670 ) ;
#4521 = DIRECTION ( 'NONE',  ( 1.000000000000000000, 0.000000000000000000, 0.000000000000000000 ) ) ;
#4522 = EDGE_CURVE ( 'NONE', #13461, #12188, #4490, .T. ) ;
#4523 = CARTESIAN_POINT ( 'NONE',  ( 93.00000000000000000, 8.660254037844390851, 205.0000000000000284 ) ) ;
#4524 =( NAMED_UNIT ( * ) PLANE_ANGLE_UNIT ( ) SI_UNIT ( $, .RADIAN. ) );
#4525 = DIRECTION ( 'NONE',  ( 0.000000000000000000, 1.000000000000000000, 0.000000000000000000 ) ) ;
#4526 = CIRCLE ( 'NONE', #1727, 2.500000000000002220 ) ;
#4527 = VERTEX_POINT ( 'NONE', #9851 ) ;
#4528 = CIRCLE ( 'NONE', #12618, 5.000000000000004441 ) ;
#4529 = ORIENTED_EDGE ( 'NONE', *, *, #4426, .F. ) ;
#4530 = DIRECTION ( 'NONE',  ( 1.000000000000000000, 0.000000000000000000, 0.000000000000000000 ) ) ;
#4531 = ORIENTED_EDGE ( 'NONE', *, *, #1798, .F. ) ;
#4532 = LINE ( 'NONE', #3451, #13807 ) ;
#4533 = ADVANCED_FACE ( 'NONE', ( #13257 ), #9925, .F. ) ;
#4534 = PLANE ( 'NONE',  #1769 ) ;
#4535 = EDGE_CURVE ( 'NONE', #11936, #11113, #8762, .T. ) ;
#4536 = CYLINDRICAL_SURFACE ( 'NONE', #8049, 2.649999999999985700 ) ;
#4537 = DIRECTION ( 'NONE',  ( 0.000000000000000000, 0.000000000000000000, -1.000000000000000000 ) ) ;
#4538 = DIRECTION ( 'NONE',  ( -0.000000000000000000, -0.000000000000000000, -1.000000000000000000 ) ) ;
#4539 = DIRECTION ( 'NONE',  ( -0.8949343913984706411, 0.4461977533473793223, 0.000000000000000000 ) ) ;
#4540 = CARTESIAN_POINT ( 'NONE',  ( 25.00000000000000000, 0.000000000000000000, 2.055000000000000160 ) ) ;
#4541 = EDGE_CURVE ( 'NONE', #3582, #4579, #9998, .T. ) ;
#4542 = ORIENTED_EDGE ( 'NONE', *, *, #2616, .F. ) ;
#4543 = DIRECTION ( 'NONE',  ( 1.000000000000000000, 0.000000000000000000, 0.000000000000000000 ) ) ;
#4544 = EDGE_CURVE ( 'NONE', #12208, #4429, #7624, .T. ) ;
#4545 = CARTESIAN_POINT ( 'NONE',  ( 8.000000000000000000, -4.837354856632045452E-15, -0.5150000000000000133 ) ) ;
#4546 = CARTESIAN_POINT ( 'NONE',  ( -5.000000000000000888, -8.660254037844389075, 210.0000000000000000 ) ) ;
#4547 = ORIENTED_EDGE ( 'NONE', *, *, #13997, .F. ) ;
#4548 = CIRCLE ( 'NONE', #11964, 10.20000000000000107 ) ;
#4549 = DIRECTION ( 'NONE',  ( -1.000000000000000000, -0.000000000000000000, -0.000000000000000000 ) ) ;
#4550 = CIRCLE ( 'NONE', #9417, 2.500000000000000444 ) ;
#4551 = DIRECTION ( 'NONE',  ( 0.000000000000000000, -0.4999999999999993894, 0.8660254037844389297 ) ) ;
#4552 = CARTESIAN_POINT ( 'NONE',  ( 53.33333333333330017, -30.00000000000000355, 222.5000000000000853 ) ) ;
#4553 =( REPRESENTATION_RELATIONSHIP ('NONE','NONE', #11251, #13104 ) REPRESENTATION_RELATIONSHIP_WITH_TRANSFORMATION ( #4627 )SHAPE_REPRESENTATION_RELATIONSHIP( ) );
#4554 = EDGE_CURVE ( 'NONE', #1188, #8138, #3341, .T. ) ;
#4555 = AXIS2_PLACEMENT_3D ( 'NONE', #10500, #9340, #7154 ) ;
#4556 = EDGE_CURVE ( 'NONE', #11681, #247, #10412, .T. ) ;
#4557 = ORIENTED_EDGE ( 'NONE', *, *, #5616, .F. ) ;
#4558 = AXIS2_PLACEMENT_3D ( 'NONE', #3467, #11091, #5640 ) ;
#4559 = DIRECTION ( 'NONE',  ( -0.000000000000000000, -0.000000000000000000, -1.000000000000000000 ) ) ;
#4560 = VECTOR ( 'NONE', #9414, 1000.000000000000000 ) ;
#4561 = ORIENTED_EDGE ( 'NONE', *, *, #7513, .F. ) ;
#4562 = CARTESIAN_POINT ( 'NONE',  ( 142.6500000000000057, -75.00000000000008527, -186.2999999999999829 ) ) ;
#4563 = ADVANCED_FACE ( 'NONE', ( #6800 ), #11225, .F. ) ;
#4564 = VECTOR ( 'NONE', #3156, 1000.000000000000000 ) ;
#4565 = VERTEX_POINT ( 'NONE', #7595 ) ;
#4566 = ORIENTED_EDGE ( 'NONE', *, *, #8079, .T. ) ;
#4567 = CARTESIAN_POINT ( 'NONE',  ( 0.000000000000000000, 0.000000000000000000, 186.0000000000000000 ) ) ;
#4568 = DIRECTION ( 'NONE',  ( 0.000000000000000000, 0.000000000000000000, 1.000000000000000000 ) ) ;
#4569 = DIRECTION ( 'NONE',  ( 0.000000000000000000, -0.000000000000000000, -1.000000000000000000 ) ) ;
#4570 = CARTESIAN_POINT ( 'NONE',  ( 140.0000000000000000, -95.00000000000008527, -186.2999999999999829 ) ) ;
#4571 = AXIS2_PLACEMENT_3D ( 'NONE', #8341, #9223, #9299 ) ;
#4572 = CARTESIAN_POINT ( 'NONE',  ( 259.0000000000000000, -8.660254037844389075, 205.0000000000000284 ) ) ;
#4573 = FACE_OUTER_BOUND ( 'NONE', #11043, .T. ) ;
#4574 = DIRECTION ( 'NONE',  ( -1.000000000000000000, -0.000000000000000000, -0.000000000000000000 ) ) ;
#4575 = CONTEXT_DEPENDENT_SHAPE_REPRESENTATION ( #8998, #8191 ) ;
#4576 = AXIS2_PLACEMENT_3D ( 'NONE', #3082, #4018, #10837 ) ;
#4577 = AXIS2_PLACEMENT_3D ( 'NONE', #1012, #5668, #3505 ) ;
#4578 = ORIENTED_EDGE ( 'NONE', *, *, #2678, .F. ) ;
#4579 = VERTEX_POINT ( 'NONE', #12031 ) ;
#4580 = CYLINDRICAL_SURFACE ( 'NONE', #9387, 2.500000000000002220 ) ;
#4581 = AXIS2_PLACEMENT_3D ( 'NONE', #9756, #10915, #13230 ) ;
#4582 = VERTEX_POINT ( 'NONE', #2085 ) ;
#4583 = DIRECTION ( 'NONE',  ( 0.000000000000000000, 0.000000000000000000, 1.000000000000000000 ) ) ;
#4584 = VECTOR ( 'NONE', #4288, 1000.000000000000000 ) ;
#4585 = VERTEX_POINT ( 'NONE', #10949 ) ;
#4586 = FACE_OUTER_BOUND ( 'NONE', #14222, .T. ) ;
#4587 = VERTEX_POINT ( 'NONE', #3262 ) ;
#4588 = DIRECTION ( 'NONE',  ( 0.000000000000000000, 0.000000000000000000, -1.000000000000000000 ) ) ;
#4589 = AXIS2_PLACEMENT_3D ( 'NONE', #5809, #10234, #5736 ) ;
#4590 = CYLINDRICAL_SURFACE ( 'NONE', #10841, 2.649999999999985700 ) ;
#4591 = DIRECTION ( 'NONE',  ( -0.000000000000000000, -0.000000000000000000, 1.000000000000000000 ) ) ;
#4592 = EDGE_CURVE ( 'NONE', #6044, #8157, #7664, .T. ) ;
#4593 = CARTESIAN_POINT ( 'NONE',  ( 386.6666666666666288, -20.00000000000000000, 225.1500000000000625 ) ) ;
#4594 = SURFACE_STYLE_USAGE ( .BOTH. , #11335 ) ;
#4595 = DIRECTION ( 'NONE',  ( 0.000000000000000000, -0.000000000000000000, 1.000000000000000000 ) ) ;
#4596 = DIRECTION ( 'NONE',  ( 1.000000000000000000, 0.000000000000000000, 0.000000000000000000 ) ) ;
#4597 = ORIENTED_EDGE ( 'NONE', *, *, #4642, .T. ) ;
#4598 = AXIS2_PLACEMENT_3D ( 'NONE', #12874, #4178, #3104 ) ;
#4599 = ORIENTED_EDGE ( 'NONE', *, *, #9, .T. ) ;
#4600 = ORIENTED_EDGE ( 'NONE', *, *, #1917, .F. ) ;
#4601 = CARTESIAN_POINT ( 'NONE',  ( 4.000000000000003553, -2.309401076758513138, -3.504271511727127031 ) ) ;
#4602 = VERTEX_POINT ( 'NONE', #13524 ) ;
#4603 = CARTESIAN_POINT ( 'NONE',  ( -2.344047193898593395, -3.265465875126480455, -1.054683074273691752E-14 ) ) ;
#4604 = LINE ( 'NONE', #4749, #11744 ) ;
#4605 = EDGE_CURVE ( 'NONE', #13503, #514, #2440, .T. ) ;
#4606 = DIRECTION ( 'NONE',  ( 0.000000000000000000, 0.000000000000000000, 1.000000000000000000 ) ) ;
#4607 = CARTESIAN_POINT ( 'NONE',  ( 4.000000000000000888, 0.8228435280416209752, -3.430609588141487976 ) ) ;
#4608 = AXIS2_PLACEMENT_3D ( 'NONE', #9810, #12262, #6539 ) ;
#4609 = PLANE ( 'NONE',  #8805 ) ;
#4610 = PRODUCT_DEFINITION_SHAPE ( 'NONE', 'NONE',  #5767 ) ;
#4611 = CARTESIAN_POINT ( 'NONE',  ( 136.6666666666666288, -25.00000000000000000, 225.1500000000000625 ) ) ;
#4612 = ADVANCED_FACE ( 'NONE', ( #300 ), #13644, .T. ) ;
#4613 = CIRCLE ( 'NONE', #7503, 0.8509999999999999787 ) ;
#4614 = VERTEX_POINT ( 'NONE', #9338 ) ;
#4615 = EDGE_CURVE ( 'NONE', #11692, #13924, #12270, .T. ) ;
#4616 = APPLICATION_CONTEXT ( 'automotive_design' ) ;
#4617 = DIRECTION ( 'NONE',  ( 0.000000000000000000, 0.000000000000000000, 1.000000000000000000 ) ) ;
#4618 = CIRCLE ( 'NONE', #1596, 2.649999999999985700 ) ;
#4619 = CARTESIAN_POINT ( 'NONE',  ( -30.00000000000002842, -225.0000000000000000, -190.0000000000000000 ) ) ;
#4620 = LINE ( 'NONE', #10197, #8516 ) ;
#4621 = ORIENTED_EDGE ( 'NONE', *, *, #2153, .T. ) ;
#4622 = CARTESIAN_POINT ( 'NONE',  ( 236.4999999999999432, -85.00000000000007105, 55.00000000000001421 ) ) ;
#4623 = PLANE ( 'NONE',  #6927 ) ;
#4624 = DIRECTION ( 'NONE',  ( -1.000000000000000000, -6.123233995736766036E-17, -6.123233995736764803E-17 ) ) ;
#4625 = AXIS2_PLACEMENT_3D ( 'NONE', #10263, #290, #1541 ) ;
#4626 = ADVANCED_FACE ( 'NONE', ( #1340 ), #10175, .F. ) ;
#4627 = ITEM_DEFINED_TRANSFORMATION ( 'NONE', 'NONE', #8380,  #14039 ) ;
#4628 = ADVANCED_FACE ( 'NONE', ( #8088 ), #4623, .T. ) ;
#4629 = CIRCLE ( 'NONE', #2549, 10.00000000000000000 ) ;
#4630 = EDGE_LOOP ( 'NONE', ( #4865, #2753, #7965, #4272 ) ) ;
#4631 = LINE ( 'NONE', #10140, #4411 ) ;
#4632 = EDGE_LOOP ( 'NONE', ( #2526, #927, #7833, #10777 ) ) ;
#4633 = ADVANCED_FACE ( 'NONE', ( #2519 ), #12523, .F. ) ;
#4634 = CARTESIAN_POINT ( 'NONE',  ( 4.236525694536557474, -2.416953475386482530, -3.751298745799839462 ) ) ;
#4635 = ORIENTED_EDGE ( 'NONE', *, *, #6061, .F. ) ;
#4636 = ORIENTED_EDGE ( 'NONE', *, *, #10938, .F. ) ;
#4637 = DIRECTION ( 'NONE',  ( -0.000000000000000000, -0.000000000000000000, 1.000000000000000000 ) ) ;
#4638 = EDGE_CURVE ( 'NONE', #145, #8138, #2656, .T. ) ;
#4639 = EDGE_CURVE ( 'NONE', #2397, #11069, #10201, .T. ) ;
#4640 = CARTESIAN_POINT ( 'NONE',  ( 2.500000000000000000, 2.357898499370433054, -1.951563910473907981E-15 ) ) ;
#4641 = DIRECTION ( 'NONE',  ( -1.000000000000000000, -0.000000000000000000, -0.000000000000000000 ) ) ;
#4642 = EDGE_CURVE ( 'NONE', #2814, #3317, #4618, .T. ) ;
#4643 = ADVANCED_FACE ( 'NONE', ( #3678 ), #2736, .T. ) ;
#4644 = VECTOR ( 'NONE', #13052, 1000.000000000000000 ) ;
#4645 = CARTESIAN_POINT ( 'NONE',  ( 140.0000000000000000, -95.00000000000008527, -190.0000000000000000 ) ) ;
#4646 = DIRECTION ( 'NONE',  ( 1.000000000000000000, 0.000000000000000000, 0.000000000000000000 ) ) ;
#4647 = CARTESIAN_POINT ( 'NONE',  ( 20.00000000000000000, 2.449293598294706513E-15, -190.0000000000000000 ) ) ;
#4648 =( NAMED_UNIT ( * ) PLANE_ANGLE_UNIT ( ) SI_UNIT ( $, .RADIAN. ) );
#4649 = AXIS2_PLACEMENT_3D ( 'NONE', #4930, #9354, #13833 ) ;
#4650 = CARTESIAN_POINT ( 'NONE',  ( 4.197393957002303999, -0.4069871074557456780, -3.503767560748925813 ) ) ;
#4651 = CONTEXT_DEPENDENT_SHAPE_REPRESENTATION ( #2051, #11006 ) ;
#4652 = VERTEX_POINT ( 'NONE', #10344 ) ;
#4653 = ORIENTED_EDGE ( 'NONE', *, *, #12321, .F. ) ;
#4654 = LINE ( 'NONE', #11394, #8690 ) ;
#4655 = CONICAL_SURFACE ( 'NONE', #4221, 2.500000000000002220, 1.029744260000002631 ) ;
#4656 = EDGE_LOOP ( 'NONE', ( #8216, #3245, #3755, #8712 ) ) ;
#4657 = AXIS2_PLACEMENT_3D ( 'NONE', #7054, #11084, #4483 ) ;
#4658 = DIRECTION ( 'NONE',  ( 0.000000000000000000, 0.000000000000000000, 1.000000000000000000 ) ) ;
#4659 = VERTEX_POINT ( 'NONE', #7076 ) ;
#4660 = DIRECTION ( 'NONE',  ( 0.000000000000000000, 0.000000000000000000, 1.000000000000000000 ) ) ;
#4661 = ORIENTED_EDGE ( 'NONE', *, *, #7816, .T. ) ;
#4662 = LINE ( 'NONE', #7838, #11260 ) ;
#4663 = CARTESIAN_POINT ( 'NONE',  ( 0.2500000000000002220, 0.000000000000000000, 4.000000000000000000 ) ) ;
#4664 = CARTESIAN_POINT ( 'NONE',  ( -140.0000000000000000, -95.00000000000008527, 30.00000000000000000 ) ) ;
#4665 = DIRECTION ( 'NONE',  ( -1.000000000000000000, 0.000000000000000000, 0.000000000000000000 ) ) ;
#4666 = AXIS2_PLACEMENT_3D ( 'NONE', #1260, #1333, #5696 ) ;
#4667 = DIRECTION ( 'NONE',  ( 0.000000000000000000, -0.000000000000000000, -1.000000000000000000 ) ) ;
#4668 = PRODUCT_CONTEXT ( 'NONE', #9538, 'mechanical' ) ;
#4669 = LINE ( 'NONE', #5675, #10599 ) ;
#4670 = ORIENTED_EDGE ( 'NONE', *, *, #5608, .T. ) ;
#4671 = CIRCLE ( 'NONE', #12768, 2.500000000000002220 ) ;
#4672 = ORIENTED_EDGE ( 'NONE', *, *, #13115, .F. ) ;
#4673 = ORIENTED_EDGE ( 'NONE', *, *, #6797, .F. ) ;
#4674 = ADVANCED_FACE ( 'NONE', ( #11508 ), #376, .T. ) ;
#4675 = LINE ( 'NONE', #8331, #2389 ) ;
#4676 = AXIS2_PLACEMENT_3D ( 'NONE', #10113, #4537, #2359 ) ;
#4677 = ORIENTED_EDGE ( 'NONE', *, *, #5239, .F. ) ;
#4678 = CYLINDRICAL_SURFACE ( 'NONE', #838, 4.250000000000000000 ) ;
#4679 = EDGE_LOOP ( 'NONE', ( #13143, #1992, #5190 ) ) ;
#4680 = DIRECTION ( 'NONE',  ( 0.000000000000000000, -0.000000000000000000, 1.000000000000000000 ) ) ;
#4681 = AXIS2_PLACEMENT_3D ( 'NONE', #13185, #6801, #11226 ) ;
#4682 = FILL_AREA_STYLE_COLOUR ( '', #8527 ) ;
#4683 = DIRECTION ( 'NONE',  ( -1.000000000000000000, -0.000000000000000000, -0.000000000000000000 ) ) ;
#4684 = DIRECTION ( 'NONE',  ( -1.000000000000000000, -0.000000000000000000, -0.000000000000000000 ) ) ;
#4685 = CARTESIAN_POINT ( 'NONE',  ( 3.678949249685231848, 0.000000000000000000, 0.000000000000000000 ) ) ;
#4686 = AXIS2_PLACEMENT_3D ( 'NONE', #9244, #579, #8364 ) ;
#4687 = CARTESIAN_POINT ( 'NONE',  ( -132.3499999999999943, 45.00000000000001421, 40.00000000000000000 ) ) ;
#4688 = AXIS2_PLACEMENT_3D ( 'NONE', #10810, #9724, #14127 ) ;
#4689 = VERTEX_POINT ( 'NONE', #11578 ) ;
#4690 = AXIS2_PLACEMENT_3D ( 'NONE', #11948, #6359, #5284 ) ;
#4691 = AXIS2_PLACEMENT_3D ( 'NONE', #5807, #2335, #10232 ) ;
#4692 = SURFACE_SIDE_STYLE ('',( #13594 ) ) ;
#4693 = DIRECTION ( 'NONE',  ( 1.000000000000000000, 0.000000000000000000, 0.000000000000000000 ) ) ;
#4694 = CARTESIAN_POINT ( 'NONE',  ( 0.000000000000000000, 0.000000000000000000, -200.0000000000000000 ) ) ;
#4695 = VECTOR ( 'NONE', #3809, 1000.000000000000000 ) ;
#4696 = DIRECTION ( 'NONE',  ( 0.000000000000000000, 1.000000000000000000, 0.000000000000000000 ) ) ;
#4697 = ORIENTED_EDGE ( 'NONE', *, *, #13243, .T. ) ;
#4698 = ADVANCED_FACE ( 'NONE', ( #5703, #4845 ), #451, .T. ) ;
#4699 = B_SPLINE_CURVE_WITH_KNOTS ( 'NONE', 3,
 ( #9224, #6829, #4952, #1516, #13711, #6029 ),
 .UNSPECIFIED., .F., .F.,
 ( 4, 2, 4 ),
 ( 0.000000000000000000, 0.0002095117440864791795, 0.0004190234881729583589 ),
 .UNSPECIFIED. ) ;
#4700 = LINE ( 'NONE', #2034, #2500 ) ;
#4701 = COLOUR_RGB ( '',1.000000000000000000, 0.9490196078431372140, 0.9098039215686274384 ) ;
#4702 = DIRECTION ( 'NONE',  ( -0.000000000000000000, 0.000000000000000000, 1.000000000000000000 ) ) ;
#4703 = CIRCLE ( 'NONE', #963, 2.700000000000000178 ) ;
#4704 = CARTESIAN_POINT ( 'NONE',  ( 0.000000000000000000, 2.349999999999998312, -0.5150000000000000133 ) ) ;
#4705 = DIRECTION ( 'NONE',  ( 6.123233995736766036E-17, -1.000000000000000000, 0.000000000000000000 ) ) ;
#4707 = AXIS2_PLACEMENT_3D ( 'NONE', #11910, #2914, #13995 ) ;
#4706 = VECTOR ( 'NONE', #11868, 1000.000000000000000 ) ;
#4708 = ORIENTED_EDGE ( 'NONE', *, *, #613, .T. ) ;
#4709 = CARTESIAN_POINT ( 'NONE',  ( 210.0000000000000000, -85.00000000000007105, 170.0000000000000000 ) ) ;
#4710 = DIRECTION ( 'NONE',  ( 0.000000000000000000, 0.000000000000000000, 1.000000000000000000 ) ) ;
#4711 = ORIENTED_EDGE ( 'NONE', *, *, #1343, .T. ) ;
#4712 = CARTESIAN_POINT ( 'NONE',  ( 3.522875095019493141, -2.820352903225631369, -3.598441714920572299 ) ) ;
#4713 = ORIENTED_EDGE ( 'NONE', *, *, #7204, .F. ) ;
#4714 = ORIENTED_EDGE ( 'NONE', *, *, #2329, .F. ) ;
#4716 = EDGE_CURVE ( 'NONE', #12934, #9938, #3537, .T. ) ;
#4715 = DIRECTION ( 'NONE',  ( 0.000000000000000000, -0.000000000000000000, 1.000000000000000000 ) ) ;
#4717 = CARTESIAN_POINT ( 'NONE',  ( -2.836893136758495970, -3.208949435745868328, -3.505054077164885484 ) ) ;
#4718 = CARTESIAN_POINT ( 'NONE',  ( 53.33333333333330017, -20.00000000000000000, 219.8500000000001080 ) ) ;
#4719 = CYLINDRICAL_SURFACE ( 'NONE', #7653, 5.500000000000005329 ) ;
#4720 = DIRECTION ( 'NONE',  ( -0.000000000000000000, -0.000000000000000000, 1.000000000000000000 ) ) ;
#4721 = CYLINDRICAL_SURFACE ( 'NONE', #5948, 2.649999999999985700 ) ;
#4722 = CARTESIAN_POINT ( 'NONE',  ( 5.200000000000002842, 3.061616997868383634E-16, -2.500000000000000444 ) ) ;
#4723 = VERTEX_POINT ( 'NONE', #6863 ) ;
#4724 = EDGE_LOOP ( 'NONE', ( #6818, #12742, #12362, #6874 ) ) ;
#4725 = EDGE_CURVE ( 'NONE', #11608, #13122, #6473, .T. ) ;
#4726 = EDGE_CURVE ( 'NONE', #7747, #9211, #6710, .T. ) ;
#4727 = LINE ( 'NONE', #1291, #5452 ) ;
#4728 = VERTEX_POINT ( 'NONE', #3894 ) ;
#4729 = ADVANCED_FACE ( 'NONE', ( #1704 ), #10644, .T. ) ;
#4730 = CARTESIAN_POINT ( 'NONE',  ( 299.9999999999999432, -75.00000000000008527, -190.0000000000000000 ) ) ;
#4731 = ORIENTED_EDGE ( 'NONE', *, *, #14182, .T. ) ;
#4732 = LINE ( 'NONE', #10161, #3197 ) ;
#4733 = EDGE_LOOP ( 'NONE', ( #12124, #570 ) ) ;
#4734 = FACE_OUTER_BOUND ( 'NONE', #3292, .T. ) ;
#4735 = DIRECTION ( 'NONE',  ( 0.000000000000000000, 0.000000000000000000, -1.000000000000000000 ) ) ;
#4736 = ORIENTED_EDGE ( 'NONE', *, *, #11567, .T. ) ;
#4737 = LINE ( 'NONE', #1590, #13648 ) ;
#4738 = CARTESIAN_POINT ( 'NONE',  ( 197.5000000000000000, -80.00000000000007105, 55.00000000000001421 ) ) ;
#4739 = APPLICATION_PROTOCOL_DEFINITION ( 'draft international standard', 'automotive_design', 1998, #3148 ) ;
#4740 = PLANE ( 'NONE',  #3193 ) ;
#4741 = EDGE_LOOP ( 'NONE', ( #1210, #14306, #6014, #8045 ) ) ;
#4742 = ORIENTED_EDGE ( 'NONE', *, *, #2253, .F. ) ;
#4743 = EDGE_CURVE ( 'NONE', #5437, #9732, #5208, .T. ) ;
#4744 = EDGE_LOOP ( 'NONE', ( #8129, #12177, #8340, #12813 ) ) ;
#4745 = DIRECTION ( 'NONE',  ( 0.000000000000000000, -1.000000000000000000, 0.000000000000000000 ) ) ;
#4746 = ORIENTED_EDGE ( 'NONE', *, *, #3117, .F. ) ;
#4747 = DIRECTION ( 'NONE',  ( -0.000000000000000000, 0.000000000000000000, -1.000000000000000000 ) ) ;
#4748 = EDGE_LOOP ( 'NONE', ( #11009, #5909 ) ) ;
#4749 = CARTESIAN_POINT ( 'NONE',  ( -5.000000000000000888, 0.000000000000000000, 200.0000000000000000 ) ) ;
#4750 = EDGE_CURVE ( 'NONE', #3217, #1051, #8158, .T. ) ;
#4751 = CARTESIAN_POINT ( 'NONE',  ( 144.9999999999999716, -64.99999999999997158, 10.00000000000000000 ) ) ;
#4752 =( REPRESENTATION_RELATIONSHIP ('NONE','NONE', #11251, #7730 ) REPRESENTATION_RELATIONSHIP_WITH_TRANSFORMATION ( #5224 )SHAPE_REPRESENTATION_RELATIONSHIP( ) );
#4753 = CARTESIAN_POINT ( 'NONE',  ( 0.3198814748697593746, 4.434118497892183264, -0.3507732604232499107 ) ) ;
#4754 = DIRECTION ( 'NONE',  ( 0.000000000000000000, 0.000000000000000000, 1.000000000000000000 ) ) ;
#4755 = DIRECTION ( 'NONE',  ( -1.000000000000000000, 0.000000000000000000, 0.000000000000000000 ) ) ;
#4756 = CARTESIAN_POINT ( 'NONE',  ( 16.55500000000001393, 0.000000000000000000, 0.000000000000000000 ) ) ;
#4757 = DIRECTION ( 'NONE',  ( 1.000000000000000000, 0.000000000000000000, 0.000000000000000000 ) ) ;
#4758 = ORIENTED_EDGE ( 'NONE', *, *, #4725, .T. ) ;
#4759 = AXIS2_PLACEMENT_3D ( 'NONE', #5349, #7789, #4261 ) ;
#4760 = DIRECTION ( 'NONE',  ( 0.000000000000000000, 3.490239007934759657E-15, -1.000000000000000000 ) ) ;
#4761 = DIRECTION ( 'NONE',  ( 0.000000000000000000, 0.000000000000000000, -1.000000000000000000 ) ) ;
#4762 = FACE_OUTER_BOUND ( 'NONE', #8447, .T. ) ;
#4763 = EDGE_LOOP ( 'NONE', ( #1653, #5160, #10543, #904 ) ) ;
#4764 = DIRECTION ( 'NONE',  ( 0.000000000000000000, 0.000000000000000000, 1.000000000000000000 ) ) ;
#4765 = EDGE_CURVE ( 'NONE', #1881, #11495, #7399, .T. ) ;
#4766 = VECTOR ( 'NONE', #4450, 1000.000000000000000 ) ;
#4767 = DIRECTION ( 'NONE',  ( -1.000000000000000000, -0.000000000000000000, -0.000000000000000000 ) ) ;
#4768 = CARTESIAN_POINT ( 'NONE',  ( 352.0000000000000000, 0.000000000000000000, 0.000000000000000000 ) ) ;
#4769 = VECTOR ( 'NONE', #3474, 1000.000000000000114 ) ;
#4770 = CARTESIAN_POINT ( 'NONE',  ( 5.200000000000002842, 0.000000000000000000, 0.000000000000000000 ) ) ;
#4771 = ORIENTED_EDGE ( 'NONE', *, *, #8080, .F. ) ;
#4772 = DIRECTION ( 'NONE',  ( 0.000000000000000000, 0.000000000000000000, -1.000000000000000000 ) ) ;
#4773 = ORIENTED_EDGE ( 'NONE', *, *, #2959, .F. ) ;
#4774 = DIRECTION ( 'NONE',  ( -0.000000000000000000, -0.000000000000000000, 1.000000000000000000 ) ) ;
#4775 = CIRCLE ( 'NONE', #4085, 2.649999999999985700 ) ;
#4776 = ORIENTED_EDGE ( 'NONE', *, *, #2621, .F. ) ;
#4777 = ORIENTED_EDGE ( 'NONE', *, *, #4200, .T. ) ;
#4778 = DIRECTION ( 'NONE',  ( 0.000000000000000000, -0.000000000000000000, 1.000000000000000000 ) ) ;
#4779 = AXIS2_PLACEMENT_3D ( 'NONE', #7239, #13902, #11666 ) ;
#4780 = DIRECTION ( 'NONE',  ( -1.000000000000000000, -0.000000000000000000, -0.000000000000000000 ) ) ;
#4781 = CARTESIAN_POINT ( 'NONE',  ( 4.000000000000000000, -2.309401076758514915, -5.000000000000000000 ) ) ;
#4782 = LINE ( 'NONE', #6951, #212 ) ;
#4783 = CYLINDRICAL_SURFACE ( 'NONE', #6286, 13.50000000000000000 ) ;
#4784 = CARTESIAN_POINT ( 'NONE',  ( 53.33333333333330017, -20.00000000000000000, 225.1500000000000625 ) ) ;
#4785 = AXIS2_PLACEMENT_3D ( 'NONE', #7078, #10346, #1483 ) ;
#4786 = CARTESIAN_POINT ( 'NONE',  ( 5.200000000000002842, 0.000000000000000000, 0.000000000000000000 ) ) ;
#4787 = CIRCLE ( 'NONE', #9919, 4.749999999999999112 ) ;
#4788 = AXIS2_PLACEMENT_3D ( 'NONE', #10873, #9568, #13040 ) ;
#4789 = VERTEX_POINT ( 'NONE', #8529 ) ;
#4790 = EDGE_LOOP ( 'NONE', ( #12382, #8039, #7229, #6257, #5294 ) ) ;
#4791 = EDGE_CURVE ( 'NONE', #4280, #9652, #5330, .T. ) ;
#4792 = VECTOR ( 'NONE', #8065, 1000.000000000000000 ) ;
#4793 = DIRECTION ( 'NONE',  ( -1.000000000000000000, -0.000000000000000000, -0.000000000000000000 ) ) ;
#4794 = EDGE_CURVE ( 'NONE', #1770, #1008, #1836, .T. ) ;
#4795 = ORIENTED_EDGE ( 'NONE', *, *, #3739, .F. ) ;
#4796 = LINE ( 'NONE', #13345, #8149 ) ;
#4797 = ORIENTED_EDGE ( 'NONE', *, *, #9370, .T. ) ;
#4798 = LINE ( 'NONE', #12554, #8979 ) ;
#4799 = ORIENTED_EDGE ( 'NONE', *, *, #1343, .F. ) ;
#4800 = CARTESIAN_POINT ( 'NONE',  ( -5.000000000000000888, 8.660254037844390851, 210.0000000000000000 ) ) ;
#4801 = VECTOR ( 'NONE', #11055, 1000.000000000000000 ) ;
#4802 = CARTESIAN_POINT ( 'NONE',  ( -304.9999999999999432, 45.00000000000001421, 30.00000000000000000 ) ) ;
#4803 = EDGE_LOOP ( 'NONE', ( #13174, #1351 ) ) ;
#4804 = DIRECTION ( 'NONE',  ( -0.000000000000000000, -0.000000000000000000, 1.000000000000000000 ) ) ;
#4805 = EDGE_CURVE ( 'NONE', #12113, #5384, #13891, .T. ) ;
#4806 = VECTOR ( 'NONE', #1581, 1000.000000000000000 ) ;
#4807 = CARTESIAN_POINT ( 'NONE',  ( 4.203833317240879275, 1.627343821129582979, -3.597273115243889929 ) ) ;
#4808 = AXIS2_PLACEMENT_3D ( 'NONE', #1374, #2765, #1513 ) ;
#4809 = DIRECTION ( 'NONE',  ( -0.000000000000000000, 1.000000000000000000, 0.000000000000000000 ) ) ;
#4810 = PRODUCT_CONTEXT ( 'NONE', #1355, 'mechanical' ) ;
#4811 = FACE_BOUND ( 'NONE', #14009, .T. ) ;
#4812 = VECTOR ( 'NONE', #494, 1000.000000000000000 ) ;
#4813 = ORIENTED_EDGE ( 'NONE', *, *, #4126, .F. ) ;
#4814 = ADVANCED_FACE ( 'NONE', ( #1627 ), #5066, .T. ) ;
#4815 = ORIENTED_EDGE ( 'NONE', *, *, #5573, .T. ) ;
#4816 = CIRCLE ( 'NONE', #2027, 13.50000000000000000 ) ;
#4817 = ORIENTED_EDGE ( 'NONE', *, *, #5553, .T. ) ;
#4818 = CARTESIAN_POINT ( 'NONE',  ( 132.4999999999999432, -56.99999999999997158, -180.0000000000000000 ) ) ;
#4819 = TOROIDAL_SURFACE ( 'NONE', #13825, 2.700000000000000622, 0.2000000000000000111 ) ;
#4820 = AXIS2_PLACEMENT_3D ( 'NONE', #9802, #7607, #13199 ) ;
#4821 = VERTEX_POINT ( 'NONE', #9477 ) ;
#4822 = DIRECTION ( 'NONE',  ( 0.000000000000000000, 0.000000000000000000, 1.000000000000000000 ) ) ;
#4823 = ORIENTED_EDGE ( 'NONE', *, *, #1694, .T. ) ;
#4824 = FACE_OUTER_BOUND ( 'NONE', #8526, .T. ) ;
#4825 = CARTESIAN_POINT ( 'NONE',  ( 200.8500000000000227, -85.00000000000007105, 55.00000000000001421 ) ) ;
#4826 = CARTESIAN_POINT ( 'NONE',  ( 0.000000000000000000, 0.000000000000000000, -200.0000000000000000 ) ) ;
#4827 = EDGE_CURVE ( 'NONE', #5470, #8867, #1927, .T. ) ;
#4828 = EDGE_CURVE ( 'NONE', #2437, #12064, #2070, .T. ) ;
#4829 = AXIS2_PLACEMENT_3D ( 'NONE', #901, #2084, #7380 ) ;
#4830 = FACE_OUTER_BOUND ( 'NONE', #6116, .T. ) ;
#4831 = EDGE_CURVE ( 'NONE', #10300, #9742, #5138, .T. ) ;
#4832 = EDGE_CURVE ( 'NONE', #1103, #6772, #11874, .T. ) ;
#4833 = DIRECTION ( 'NONE',  ( 0.000000000000000000, 1.224646799147353207E-16, 1.000000000000000000 ) ) ;
#4834 = AXIS2_PLACEMENT_3D ( 'NONE', #5134, #7576, #1768 ) ;
#4835 = CYLINDRICAL_SURFACE ( 'NONE', #4625, 2.649999999999985700 ) ;
#4836 = CARTESIAN_POINT ( 'NONE',  ( 1.999999999999994893, 0.000000000000000000, 0.000000000000000000 ) ) ;
#4837 = EDGE_CURVE ( 'NONE', #6422, #7082, #1367, .T. ) ;
#4838 = ORIENTED_EDGE ( 'NONE', *, *, #7993, .T. ) ;
#4839 = DIRECTION ( 'NONE',  ( -0.000000000000000000, -0.000000000000000000, 1.000000000000000000 ) ) ;
#4840 = DIRECTION ( 'NONE',  ( 0.000000000000000000, 0.000000000000000000, 1.000000000000000000 ) ) ;
#4841 = DIRECTION ( 'NONE',  ( 0.000000000000000000, -0.4999999999999992784, 0.8660254037844389297 ) ) ;
#4842 = AXIS2_PLACEMENT_3D ( 'NONE', #11565, #6054, #6197 ) ;
#4843 = ORIENTED_EDGE ( 'NONE', *, *, #8449, .T. ) ;
#4844 = FACE_OUTER_BOUND ( 'NONE', #4632, .T. ) ;
#4845 = FACE_OUTER_BOUND ( 'NONE', #2173, .T. ) ;
#4846 = DIRECTION ( 'NONE',  ( 6.123233995736766036E-17, -1.000000000000000000, 0.000000000000000000 ) ) ;
#4847 = VECTOR ( 'NONE', #5742, 1000.000000000000000 ) ;
#4848 = DIRECTION ( 'NONE',  ( -0.000000000000000000, -0.000000000000000000, 1.000000000000000000 ) ) ;
#4849 = ORIENTED_EDGE ( 'NONE', *, *, #12121, .T. ) ;
#4850 = DIRECTION ( 'NONE',  ( -1.000000000000000000, 0.000000000000000000, 0.000000000000000000 ) ) ;
#4851 = PRODUCT_DEFINITION_SHAPE ( 'NONE', 'NONE',  #12238 ) ;
#4852 = ADVANCED_FACE ( 'NONE', ( #11725 ), #6069, .F. ) ;
#4853 = DIRECTION ( 'NONE',  ( 0.000000000000000000, 0.000000000000000000, -1.000000000000000000 ) ) ;
#4854 = EDGE_LOOP ( 'NONE', ( #8838, #8501 ) ) ;
#4855 = CARTESIAN_POINT ( 'NONE',  ( 299.9999999999999432, -75.00000000000008527, -186.2999999999999829 ) ) ;
#4856 = DIRECTION ( 'NONE',  ( 0.000000000000000000, -1.000000000000000000, 0.000000000000000000 ) ) ;
#4857 = CARTESIAN_POINT ( 'NONE',  ( 2.500000000000000000, -1.178949249685213863, 2.042000000000002924 ) ) ;
#4858 = VECTOR ( 'NONE', #8307, 1000.000000000000000 ) ;
#4859 = DIRECTION ( 'NONE',  ( 1.000000000000000000, 0.000000000000000000, 0.000000000000000000 ) ) ;
#4860 = CARTESIAN_POINT ( 'NONE',  ( -3.680118525130244400, 2.494084732383327285, -0.3507732604232449702 ) ) ;
#4861 = DIRECTION ( 'NONE',  ( -0.000000000000000000, -0.000000000000000000, -1.000000000000000000 ) ) ;
#4862 = SURFACE_STYLE_USAGE ( .BOTH. , #10362 ) ;
#4863 = CARTESIAN_POINT ( 'NONE',  ( 132.3499999999999943, 45.00000000000001421, -1.230770033143087371E-15 ) ) ;
#4864 = CONTEXT_DEPENDENT_SHAPE_REPRESENTATION ( #9274, #6364 ) ;
#4865 = ORIENTED_EDGE ( 'NONE', *, *, #12279, .F. ) ;
#4866 = ORIENTED_EDGE ( 'NONE', *, *, #9865, .F. ) ;
#4867 = CARTESIAN_POINT ( 'NONE',  ( 3.700000000000000178, 0.000000000000000000, 0.000000000000000000 ) ) ;
#4868 = EDGE_CURVE ( 'NONE', #5253, #11990, #4409, .T. ) ;
#4869 = ORIENTED_EDGE ( 'NONE', *, *, #1007, .T. ) ;
#4870 = DIRECTION ( 'NONE',  ( -1.000000000000000000, -0.000000000000000000, -0.000000000000000000 ) ) ;
#4871 = VECTOR ( 'NONE', #10054, 1000.000000000000000 ) ;
#4872 = VECTOR ( 'NONE', #9268, 1000.000000000000000 ) ;
#4873 = EDGE_LOOP ( 'NONE', ( #23, #555, #6683, #2383 ) ) ;
#4874 = FACE_OUTER_BOUND ( 'NONE', #8626, .T. ) ;
#4875 = ORIENTED_EDGE ( 'NONE', *, *, #6775, .F. ) ;
#4876 = DIRECTION ( 'NONE',  ( -0.000000000000000000, -0.000000000000000000, -1.000000000000000000 ) ) ;
#4877 = CARTESIAN_POINT ( 'NONE',  ( 357.0000000000000000, 8.660254037844390851, 200.0000000000000000 ) ) ;
#4878 = ORIENTED_EDGE ( 'NONE', *, *, #11204, .T. ) ;
#4879 = VECTOR ( 'NONE', #10383, 1000.000000000000000 ) ;
#4880 = FACE_BOUND ( 'NONE', #8930, .T. ) ;
#4881 = ADVANCED_FACE ( 'NONE', ( #1855 ), #13028, .F. ) ;
#4882 = DIRECTION ( 'NONE',  ( -1.000000000000000000, -0.000000000000000000, -0.000000000000000000 ) ) ;
#4883 = LINE ( 'NONE', #3854, #12510 ) ;
#4884 = PRODUCT_CONTEXT ( 'NONE', #4152, 'mechanical' ) ;
#4885 = DIRECTION ( 'NONE',  ( 0.000000000000000000, 0.000000000000000000, 1.000000000000000000 ) ) ;
#4886 = ORIENTED_EDGE ( 'NONE', *, *, #2054, .T. ) ;
#4887 = CIRCLE ( 'NONE', #12986, 2.500000000000000888 ) ;
#4888 = FACE_BOUND ( 'NONE', #925, .T. ) ;
#4889 = ORIENTED_EDGE ( 'NONE', *, *, #10798, .F. ) ;
#4890 = CARTESIAN_POINT ( 'NONE',  ( 134.9999999999999432, -36.99999999999997868, -169.9999999999999716 ) ) ;
#4891 = EDGE_LOOP ( 'NONE', ( #7491, #9954, #11969, #2704 ) ) ;
#4892 = CARTESIAN_POINT ( 'NONE',  ( 134.5000000000000000, -95.00000000000008527, -186.2999999999999829 ) ) ;
#4893 = ORIENTED_EDGE ( 'NONE', *, *, #12085, .F. ) ;
#4894 = DIRECTION ( 'NONE',  ( -0.000000000000000000, 0.000000000000000000, -1.000000000000000000 ) ) ;
#4895 = DIRECTION ( 'NONE',  ( -0.000000000000000000, 1.000000000000000000, -0.000000000000000000 ) ) ;
#4896 = CIRCLE ( 'NONE', #12079, 2.055000000000000160 ) ;
#4897 = LINE ( 'NONE', #9318, #9440 ) ;
#4898 = EDGE_CURVE ( 'NONE', #1850, #7429, #1133, .T. ) ;
#4899 = FACE_OUTER_BOUND ( 'NONE', #9855, .T. ) ;
#4900 = VECTOR ( 'NONE', #5260, 1000.000000000000000 ) ;
#4901 = CARTESIAN_POINT ( 'NONE',  ( 140.0000000000000000, -95.00000000000008527, -186.2999999999999829 ) ) ;
#4902 = DIRECTION ( 'NONE',  ( -0.000000000000000000, -0.000000000000000000, -1.000000000000000000 ) ) ;
#4903 = ORIENTED_EDGE ( 'NONE', *, *, #13930, .T. ) ;
#4904 = ORIENTED_EDGE ( 'NONE', *, *, #234, .T. ) ;
#4905 = AXIS2_PLACEMENT_3D ( 'NONE', #7292, #5346, #6210 ) ;
#4906 = ADVANCED_FACE ( 'NONE', ( #11657 ), #5531, .F. ) ;
#4907 = EDGE_CURVE ( 'NONE', #161, #11376, #8957, .T. ) ;
#4908 = STYLED_ITEM ( 'NONE', ( #9662 ), #4041 ) ;
#4909 = EDGE_CURVE ( 'NONE', #1298, #247, #959, .T. ) ;
#4910 = CARTESIAN_POINT ( 'NONE',  ( 219.9999999999999716, -15.00000000000000000, 219.8500000000001080 ) ) ;
#4911 = CARTESIAN_POINT ( 'NONE',  ( 2.740000000000000213, 0.000000000000000000, 0.000000000000000000 ) ) ;
#4912 = VERTEX_POINT ( 'NONE', #6713 ) ;
#4913 = VECTOR ( 'NONE', #357, 1000.000000000000000 ) ;
#4914 = CYLINDRICAL_SURFACE ( 'NONE', #12436, 2.649999999999985700 ) ;
#4915 = CIRCLE ( 'NONE', #1402, 2.700000000000000622 ) ;
#4916 = COLOUR_RGB ( '',0.8941176470588234615, 0.8941176470588234615, 0.8941176470588234615 ) ;
#4917 = DIRECTION ( 'NONE',  ( 0.000000000000000000, -0.000000000000000000, 1.000000000000000000 ) ) ;
#4918 = CARTESIAN_POINT ( 'NONE',  ( 136.6666666666666288, -10.00000000000000178, -222.5000000000000853 ) ) ;
#4919 = CARTESIAN_POINT ( 'NONE',  ( 93.00000000000000000, 8.660254037844390851, 199.9990000000000236 ) ) ;
#4920 = EDGE_LOOP ( 'NONE', ( #51, #9218, #9560, #4048 ) ) ;
#4921 = LINE ( 'NONE', #13896, #5342 ) ;
#4922 = AXIS2_PLACEMENT_3D ( 'NONE', #3981, #6009, #5082 ) ;
#4923 = CARTESIAN_POINT ( 'NONE',  ( 134.9999999999999716, 45.00000000000001421, 10.00000000000000000 ) ) ;
#4924 = AXIS2_PLACEMENT_3D ( 'NONE', #9703, #14108, #10498 ) ;
#4925 =( GEOMETRIC_REPRESENTATION_CONTEXT ( 3 ) GLOBAL_UNCERTAINTY_ASSIGNED_CONTEXT ( ( #11924 ) ) GLOBAL_UNIT_ASSIGNED_CONTEXT ( ( #8462, #2822, #9489 ) ) REPRESENTATION_CONTEXT ( 'NONE', 'WORKASPACE' ) );
#4926 = VERTEX_POINT ( 'NONE', #3458 ) ;
#4927 = LINE ( 'NONE', #461, #7999 ) ;
#4928 = CARTESIAN_POINT ( 'NONE',  ( 3.472371940585993855, 2.614027278893175321, -3.320322319201766792 ) ) ;
#4929 = CARTESIAN_POINT ( 'NONE',  ( 140.0000000000000000, -95.00000000000008527, 186.2999999999999829 ) ) ;
#4930 = CARTESIAN_POINT ( 'NONE',  ( 53.33333333333330017, -20.00000000000000000, 222.5000000000000853 ) ) ;
#4931 = DIRECTION ( 'NONE',  ( -1.000000000000000000, -0.000000000000000000, -0.000000000000000000 ) ) ;
#4932 = LINE ( 'NONE', #13763, #12898 ) ;
#4934 = AXIS2_PLACEMENT_3D ( 'NONE', #8485, #13857, #10529 ) ;
#4933 = VECTOR ( 'NONE', #807, 1000.000000000000000 ) ;
#4935 = EDGE_CURVE ( 'NONE', #7052, #12248, #10864, .T. ) ;
#4936 = CYLINDRICAL_SURFACE ( 'NONE', #12256, 2.649999999999985700 ) ;
#4937 = VECTOR ( 'NONE', #12137, 999.9999999999997726 ) ;
#4938 =( GEOMETRIC_REPRESENTATION_CONTEXT ( 3 ) GLOBAL_UNCERTAINTY_ASSIGNED_CONTEXT ( ( #6530 ) ) GLOBAL_UNIT_ASSIGNED_CONTEXT ( ( #7539, #5176, #10753 ) ) REPRESENTATION_CONTEXT ( 'NONE', 'WORKASPACE' ) );
#4939 = ORIENTED_EDGE ( 'NONE', *, *, #7636, .F. ) ;
#4940 = FACE_OUTER_BOUND ( 'NONE', #3820, .T. ) ;
#4941 = ORIENTED_EDGE ( 'NONE', *, *, #8419, .T. ) ;
#4942 = DIRECTION ( 'NONE',  ( -0.000000000000000000, -0.000000000000000000, -1.000000000000000000 ) ) ;
#4943 = DIRECTION ( 'NONE',  ( -0.000000000000000000, -0.000000000000000000, -1.000000000000000000 ) ) ;
#4944 = AXIS2_PLACEMENT_3D ( 'NONE', #12762, #4942, #13844 ) ;
#4945 = ORIENTED_EDGE ( 'NONE', *, *, #7469, .T. ) ;
#4946 = CARTESIAN_POINT ( 'NONE',  ( 1.800000000000002931, 1.653273178848927261E-15, 13.50000000000000178 ) ) ;
#4947 = ORIENTED_EDGE ( 'NONE', *, *, #10119, .T. ) ;
#4948 = CARTESIAN_POINT ( 'NONE',  ( 0.000000000000000000, 0.000000000000000000, -200.0000000000000000 ) ) ;
#4949 = CARTESIAN_POINT ( 'NONE',  ( -302.4999999999999432, -75.00000000000008527, 10.00000000000000178 ) ) ;
#4950 = ORIENTED_EDGE ( 'NONE', *, *, #10400, .F. ) ;
#4951 = UNCERTAINTY_MEASURE_WITH_UNIT (LENGTH_MEASURE( 1.000000000000000082E-05 ), #9085, 'distance_accuracy_value', 'NONE');
#4952 = CARTESIAN_POINT ( 'NONE',  ( -1.149515148933674504E-15, -4.647091401871393579, -3.572172305156879890 ) ) ;
#4953 = B_SPLINE_CURVE_WITH_KNOTS ( 'NONE', 3,
 ( #14241, #13238, #1991, #5413, #8741, #3102, #11884, #12145 ),
 .UNSPECIFIED., .F., .F.,
 ( 4, 2, 2, 4 ),
 ( 0.000000000000000000, 0.002450665683189819262, 0.003675998524784728893, 0.004901331366379639391 ),
 .UNSPECIFIED. ) ;
#4954 = EDGE_CURVE ( 'NONE', #8236, #701, #8749, .T. ) ;
#4955 = LINE ( 'NONE', #10459, #4879 ) ;
#4956 = PRODUCT_CONTEXT ( 'NONE', #6096, 'mechanical' ) ;
#4957 = DIRECTION ( 'NONE',  ( -0.000000000000000000, -0.000000000000000000, 1.000000000000000000 ) ) ;
#4958 = EDGE_LOOP ( 'NONE', ( #4247, #9694, #5845, #5829 ) ) ;
#4959 = VERTEX_POINT ( 'NONE', #1995 ) ;
#4960 = ORIENTED_EDGE ( 'NONE', *, *, #11673, .F. ) ;
#4961 = CARTESIAN_POINT ( 'NONE',  ( 219.9999999999999716, -20.00000000000000000, 219.8500000000001080 ) ) ;
#4962 = ADVANCED_FACE ( 'NONE', ( #6432 ), #78, .F. ) ;
#4963 = VERTEX_POINT ( 'NONE', #2073 ) ;
#4964 = DIRECTION ( 'NONE',  ( -0.000000000000000000, 0.000000000000000000, 1.000000000000000000 ) ) ;
#4965 = ORIENTED_EDGE ( 'NONE', *, *, #1512, .T. ) ;
#4966 = FACE_BOUND ( 'NONE', #2098, .T. ) ;
#4967 = CARTESIAN_POINT ( 'NONE',  ( 0.9586399445693768451, 0.5149999999999971267, 0.8293189044373084906 ) ) ;
#4968 = CARTESIAN_POINT ( 'NONE',  ( 53.33333333333330017, -20.00000000000000000, -225.1500000000000625 ) ) ;
#4969 = FACE_OUTER_BOUND ( 'NONE', #12928, .T. ) ;
#4970 = LINE ( 'NONE', #580, #7208 ) ;
#4971 = CARTESIAN_POINT ( 'NONE',  ( 2.740000000000000213, -0.5150000000000034550, 0.9838866223909985553 ) ) ;
#4972 = PRODUCT_DEFINITION_SHAPE ( 'NONE', 'NONE',  #14336 ) ;
#4973 = ORIENTED_EDGE ( 'NONE', *, *, #11212, .T. ) ;
#4974 = VERTEX_POINT ( 'NONE', #9913 ) ;
#4975 = EDGE_CURVE ( 'NONE', #8647, #6112, #3249, .T. ) ;
#4976 =( NAMED_UNIT ( * ) SI_UNIT ( $, .STERADIAN. ) SOLID_ANGLE_UNIT ( ) );
#4977 = EDGE_CURVE ( 'NONE', #9188, #7620, #8321, .T. ) ;
#4978 = ORIENTED_EDGE ( 'NONE', *, *, #1252, .T. ) ;
#4979 = FACE_OUTER_BOUND ( 'NONE', #9904, .T. ) ;
#4980 = DIRECTION ( 'NONE',  ( 0.000000000000000000, 0.000000000000000000, -1.000000000000000000 ) ) ;
#4981 = AXIS2_PLACEMENT_3D ( 'NONE', #1965, #8863, #4228 ) ;
#4982 = DIRECTION ( 'NONE',  ( -1.000000000000000000, 0.000000000000000000, 0.000000000000000000 ) ) ;
#4983 = ORIENTED_EDGE ( 'NONE', *, *, #1110, .F. ) ;
#4984 = CARTESIAN_POINT ( 'NONE',  ( 305.4999999999999432, -95.00000000000008527, -186.2999999999999829 ) ) ;
#4985 = EDGE_CURVE ( 'NONE', #1896, #6825, #3022, .T. ) ;
#4986 = CARTESIAN_POINT ( 'NONE',  ( 219.9999999999999716, -85.00000000000007105, 64.14213562373096522 ) ) ;
#4987 = DIRECTION ( 'NONE',  ( 1.000000000000000000, 0.000000000000000000, 6.123233995736766036E-17 ) ) ;
#4988 = DIRECTION ( 'NONE',  ( 0.000000000000000000, 0.000000000000000000, 1.000000000000000000 ) ) ;
#4989 = CARTESIAN_POINT ( 'NONE',  ( 319.9999999999999432, -24.99999999999999289, 19.99999999999998934 ) ) ;
#4990 = CIRCLE ( 'NONE', #1259, 7.983406227920510467 ) ;
#4991 = ORIENTED_EDGE ( 'NONE', *, *, #9026, .T. ) ;
#4992 = EDGE_CURVE ( 'NONE', #498, #11674, #12043, .T. ) ;
#4993 = DIRECTION ( 'NONE',  ( -0.000000000000000000, -0.000000000000000000, 1.000000000000000000 ) ) ;
#4994 = CARTESIAN_POINT ( 'NONE',  ( 170.9999999999999716, -8.660254037844389075, 199.9990000000000236 ) ) ;
#4995 = ORIENTED_EDGE ( 'NONE', *, *, #4837, .T. ) ;
#4996 = CYLINDRICAL_SURFACE ( 'NONE', #1994, 2.649999999999985700 ) ;
#4997 = CARTESIAN_POINT ( 'NONE',  ( -294.9999999999999432, -75.00000000000008527, 0.000000000000000000 ) ) ;
#4998 = EDGE_CURVE ( 'NONE', #514, #8720, #1107, .T. ) ;
#4999 = CARTESIAN_POINT ( 'NONE',  ( 386.6666666666666288, -20.00000000000000000, 222.5000000000000853 ) ) ;
#5000 = CARTESIAN_POINT ( 'NONE',  ( 0.000000000000000000, 0.000000000000000000, 186.0000000000000000 ) ) ;
#5001 = FACE_OUTER_BOUND ( 'NONE', #6397, .T. ) ;
#5002 =( NAMED_UNIT ( * ) PLANE_ANGLE_UNIT ( ) SI_UNIT ( $, .RADIAN. ) );
#5003 = EDGE_CURVE ( 'NONE', #5319, #13651, #6575, .T. ) ;
#5004 = CARTESIAN_POINT ( 'NONE',  ( 4.000000000000000000, 0.000000000000000000, 0.000000000000000000 ) ) ;
#5005 = CONTEXT_DEPENDENT_SHAPE_REPRESENTATION ( #12432, #3256 ) ;
#5006 = VERTEX_POINT ( 'NONE', #8895 ) ;
#5007 = ADVANCED_FACE ( 'NONE', ( #8823 ), #9985, .T. ) ;
#5008 = CYLINDRICAL_SURFACE ( 'NONE', #13087, 5.000000000000004441 ) ;
#5009 = CIRCLE ( 'NONE', #13102, 2.500000000000002220 ) ;
#5010 = ORIENTED_EDGE ( 'NONE', *, *, #13840, .F. ) ;
#5011 = DIRECTION ( 'NONE',  ( -1.000000000000000000, -0.000000000000000000, -0.000000000000000000 ) ) ;
#5012 = FACE_OUTER_BOUND ( 'NONE', #13790, .T. ) ;
#5013 = ORIENTED_EDGE ( 'NONE', *, *, #8715, .F. ) ;
#5014 = DIRECTION ( 'NONE',  ( 0.000000000000000000, 0.000000000000000000, 1.000000000000000000 ) ) ;
#5015 = ORIENTED_EDGE ( 'NONE', *, *, #2292, .F. ) ;
#5016 = DIRECTION ( 'NONE',  ( 0.000000000000000000, 0.000000000000000000, -1.000000000000000000 ) ) ;
#5017 = LINE ( 'NONE', #10526, #11497 ) ;
#5018 = ORIENTED_EDGE ( 'NONE', *, *, #9707, .F. ) ;
#5019 = CIRCLE ( 'NONE', #2470, 2.500000000000002220 ) ;
#5020 = DIRECTION ( 'NONE',  ( 1.000000000000000000, 0.000000000000000000, 0.000000000000000000 ) ) ;
#5021 = DIRECTION ( 'NONE',  ( -1.000000000000000000, 0.000000000000000000, 0.000000000000000000 ) ) ;
#5022 = VECTOR ( 'NONE', #5581, 1000.000000000000000 ) ;
#5023 = FILL_AREA_STYLE ('',( #2699 ) ) ;
#5024 = DIRECTION ( 'NONE',  ( 1.000000000000000000, 0.000000000000000000, 0.000000000000000000 ) ) ;
#5025 = PRODUCT_CONTEXT ( 'NONE', #12581, 'mechanical' ) ;
#5026 = AXIS2_PLACEMENT_3D ( 'NONE', #10047, #70, #3381 ) ;
#5027 = CARTESIAN_POINT ( 'NONE',  ( 357.0000000000000000, -8.660254037844389075, 205.0000000000000284 ) ) ;
#5028 = VERTEX_POINT ( 'NONE', #8674 ) ;
#5029 =( REPRESENTATION_RELATIONSHIP ('NONE','NONE', #11251, #2275 ) REPRESENTATION_RELATIONSHIP_WITH_TRANSFORMATION ( #8911 )SHAPE_REPRESENTATION_RELATIONSHIP( ) );
#5030 = VERTEX_POINT ( 'NONE', #13307 ) ;
#5031 = ORIENTED_EDGE ( 'NONE', *, *, #6657, .F. ) ;
#5032 = CIRCLE ( 'NONE', #3631, 12.77500000000000036 ) ;
#5033 = ORIENTED_EDGE ( 'NONE', *, *, #9762, .F. ) ;
#5034 = CARTESIAN_POINT ( 'NONE',  ( 134.9999999999999432, -36.99999999999997868, -180.0000000000000000 ) ) ;
#5035 = AXIS2_PLACEMENT_3D ( 'NONE', #1703, #13676, #11577 ) ;
#5036 = CIRCLE ( 'NONE', #10822, 2.649999999999985700 ) ;
#5037 = EDGE_CURVE ( 'NONE', #7333, #13531, #13, .T. ) ;
#5038 = VERTEX_POINT ( 'NONE', #11000 ) ;
#5039 = CARTESIAN_POINT ( 'NONE',  ( 3.016506661494197328, 0.000000000000000000, 7.007546303702493782E-17 ) ) ;
#5040 = ORIENTED_EDGE ( 'NONE', *, *, #3468, .F. ) ;
#5041 = CARTESIAN_POINT ( 'NONE',  ( 0.000000000000000000, 0.000000000000000000, 4.000000000000000000 ) ) ;
#5042 = AXIS2_PLACEMENT_3D ( 'NONE', #2496, #502, #4964 ) ;
#5043 = PRESENTATION_STYLE_ASSIGNMENT (( #12431 ) ) ;
#5044 = DIRECTION ( 'NONE',  ( -1.000000000000000000, 0.000000000000000000, 0.000000000000000000 ) ) ;
#5045 = VECTOR ( 'NONE', #1820, 1000.000000000000000 ) ;
#5046 = CARTESIAN_POINT ( 'NONE',  ( 319.9999999999999432, -24.99999999999999289, -19.99999999999998934 ) ) ;
#5047 = LINE ( 'NONE', #358, #3962 ) ;
#5048 = AXIS2_PLACEMENT_3D ( 'NONE', #12411, #4804, #3571 ) ;
#5049 = DIRECTION ( 'NONE',  ( 0.000000000000000000, 0.000000000000000000, 1.000000000000000000 ) ) ;
#5050 = ORIENTED_EDGE ( 'NONE', *, *, #167, .T. ) ;
#5051 = AXIS2_PLACEMENT_3D ( 'NONE', #1730, #13989, #5014 ) ;
#5052 = ORIENTED_EDGE ( 'NONE', *, *, #11922, .F. ) ;
#5053 = VECTOR ( 'NONE', #13634, 1000.000000000000000 ) ;
#5054 = DIRECTION ( 'NONE',  ( -0.000000000000000000, 1.000000000000000000, -0.000000000000000000 ) ) ;
#5055 = EDGE_CURVE ( 'NONE', #4077, #232, #13884, .T. ) ;
#5056 = CIRCLE ( 'NONE', #1047, 2.041999999999999815 ) ;
#5057 = ORIENTED_EDGE ( 'NONE', *, *, #5908, .T. ) ;
#5058 = DIRECTION ( 'NONE',  ( -0.000000000000000000, 0.000000000000000000, 1.000000000000000000 ) ) ;
#5059 = DIRECTION ( 'NONE',  ( -1.000000000000000000, -0.000000000000000000, -0.000000000000000000 ) ) ;
#5060 = TOROIDAL_SURFACE ( 'NONE', #5499, 5.384454397937118664, 0.5155456020628804703 ) ;
#5061 = FACE_OUTER_BOUND ( 'NONE', #8591, .T. ) ;
#5062 = ORIENTED_EDGE ( 'NONE', *, *, #11598, .F. ) ;
#5063 = CIRCLE ( 'NONE', #1559, 7.983406227920510467 ) ;
#5064 = CARTESIAN_POINT ( 'NONE',  ( 302.5000000000000000, -56.99999999999997158, -180.0000000000000000 ) ) ;
#5065 = EDGE_CURVE ( 'NONE', #2338, #770, #12087, .T. ) ;
#5066 = CYLINDRICAL_SURFACE ( 'NONE', #8313, 5.000000000000004441 ) ;
#5067 = CARTESIAN_POINT ( 'NONE',  ( 0.000000000000000000, 0.000000000000000000, -169.9999999999999716 ) ) ;
#5068 = EDGE_CURVE ( 'NONE', #2336, #14079, #2148, .T. ) ;
#5069 = DIRECTION ( 'NONE',  ( -0.000000000000000000, -0.000000000000000000, -1.000000000000000000 ) ) ;
#5070 = CARTESIAN_POINT ( 'NONE',  ( 53.33333333333330017, -14.99999999999999822, 219.8500000000001080 ) ) ;
#5071 = ORIENTED_EDGE ( 'NONE', *, *, #872, .T. ) ;
#5072 = VECTOR ( 'NONE', #11856, 1000.000000000000000 ) ;
#5073 = DIRECTION ( 'NONE',  ( 0.000000000000000000, 1.000000000000000000, 0.000000000000000000 ) ) ;
#5074 = CARTESIAN_POINT ( 'NONE',  ( 444.9999999999999432, 8.660254037844390851, 205.0000000000000284 ) ) ;
#5075 = ORIENTED_EDGE ( 'NONE', *, *, #11318, .T. ) ;
#5076 = DIRECTION ( 'NONE',  ( 1.000000000000000000, 0.000000000000000000, 0.000000000000000000 ) ) ;
#5077 = DIRECTION ( 'NONE',  ( 1.000000000000000000, 0.000000000000000000, 0.000000000000000000 ) ) ;
#5078 = DIRECTION ( 'NONE',  ( 0.000000000000000000, 0.000000000000000000, -1.000000000000000000 ) ) ;
#5079 = ADVANCED_FACE ( 'NONE', ( #1397 ), #4835, .F. ) ;
#5080 = DIRECTION ( 'NONE',  ( 0.000000000000000000, 1.000000000000000000, 0.000000000000000000 ) ) ;
#5081 = EDGE_CURVE ( 'NONE', #663, #5230, #2507, .T. ) ;
#5082 = DIRECTION ( 'NONE',  ( 1.000000000000000000, 0.000000000000000000, 0.000000000000000000 ) ) ;
#5083 = FACE_BOUND ( 'NONE', #8608, .T. ) ;
#5084 = DIRECTION ( 'NONE',  ( -0.000000000000000000, -0.000000000000000000, 1.000000000000000000 ) ) ;
#5085 = AXIS2_PLACEMENT_3D ( 'NONE', #13044, #7458, #3047 ) ;
#5086 = ORIENTED_EDGE ( 'NONE', *, *, #12502, .T. ) ;
#5087 = DIRECTION ( 'NONE',  ( -0.000000000000000000, -0.000000000000000000, -1.000000000000000000 ) ) ;
#5088 = EDGE_LOOP ( 'NONE', ( #7598, #6594, #6457, #2690 ) ) ;
#5089 = CARTESIAN_POINT ( 'NONE',  ( 137.4999999999999716, 45.00000000000001421, 0.000000000000000000 ) ) ;
#5090 = DIRECTION ( 'NONE',  ( 0.000000000000000000, 0.000000000000000000, 1.000000000000000000 ) ) ;
#5091 = EDGE_CURVE ( 'NONE', #3111, #11223, #11281, .T. ) ;
#5092 = EDGE_CURVE ( 'NONE', #2372, #1020, #195, .T. ) ;
#5093 =( REPRESENTATION_RELATIONSHIP ('NONE','NONE', #11251, #13104 ) REPRESENTATION_RELATIONSHIP_WITH_TRANSFORMATION ( #3070 )SHAPE_REPRESENTATION_RELATIONSHIP( ) );
#5094 = ORIENTED_EDGE ( 'NONE', *, *, #7739, .F. ) ;
#5095 = EDGE_CURVE ( 'NONE', #2998, #11990, #11813, .T. ) ;
#5096 = FACE_OUTER_BOUND ( 'NONE', #5827, .T. ) ;
#5097 = ORIENTED_EDGE ( 'NONE', *, *, #1774, .T. ) ;
#5098 = CARTESIAN_POINT ( 'NONE',  ( 0.2500000000000002220, 0.000000000000000000, 0.000000000000000000 ) ) ;
#5099 = PRODUCT_DEFINITION_SHAPE ( 'NONE', 'NONE',  #14369 ) ;
#5100 = DIRECTION ( 'NONE',  ( -1.000000000000000000, 0.000000000000000000, 0.000000000000000000 ) ) ;
#5101 = EDGE_LOOP ( 'NONE', ( #13141, #5013 ) ) ;
#5102 = DIRECTION ( 'NONE',  ( 0.000000000000000000, 0.000000000000000000, 1.000000000000000000 ) ) ;
#5103 = CARTESIAN_POINT ( 'NONE',  ( -304.9999999999999432, -95.00000000000008527, 39.99999999999997868 ) ) ;
#5104 = CARTESIAN_POINT ( 'NONE',  ( 25.00000000000000000, 0.000000000000000000, 0.000000000000000000 ) ) ;
#5105 = SHAPE_DEFINITION_REPRESENTATION ( #4851, #10713 ) ;
#5106 = DIRECTION ( 'NONE',  ( 0.000000000000000000, 0.000000000000000000, 1.000000000000000000 ) ) ;
#5107 = ORIENTED_EDGE ( 'NONE', *, *, #5180, .T. ) ;
#5108 = AXIS2_PLACEMENT_3D ( 'NONE', #5984, #6994, #2362 ) ;
#5109 = ORIENTED_EDGE ( 'NONE', *, *, #1687, .T. ) ;
#5110 = CARTESIAN_POINT ( 'NONE',  ( 137.6499999999999773, 45.00000000000001421, 0.000000000000000000 ) ) ;
#5111 = EDGE_LOOP ( 'NONE', ( #10886, #4561 ) ) ;
#5112 = CIRCLE ( 'NONE', #1849, 2.649999999999985700 ) ;
#5113 = DIRECTION ( 'NONE',  ( -0.000000000000000000, 1.000000000000000000, -0.000000000000000000 ) ) ;
#5114 = AXIS2_PLACEMENT_3D ( 'NONE', #12626, #4809, #13715 ) ;
#5115 = ORIENTED_EDGE ( 'NONE', *, *, #2196, .F. ) ;
#5116 = DIRECTION ( 'NONE',  ( -1.000000000000000000, 0.000000000000000000, 0.000000000000000000 ) ) ;
#5117 = ORIENTED_EDGE ( 'NONE', *, *, #1413, .T. ) ;
#5118 = CYLINDRICAL_SURFACE ( 'NONE', #12664, 5.500000000000005329 ) ;
#5119 = DIRECTION ( 'NONE',  ( -0.000000000000000000, -0.000000000000000000, -1.000000000000000000 ) ) ;
#5120 = DIRECTION ( 'NONE',  ( 1.000000000000000000, 0.000000000000000000, 0.000000000000000000 ) ) ;
#5121 = DIRECTION ( 'NONE',  ( -0.000000000000000000, -0.000000000000000000, 1.000000000000000000 ) ) ;
#5122 = AXIS2_PLACEMENT_3D ( 'NONE', #7374, #4118, #1860 ) ;
#5123 =( NAMED_UNIT ( * ) PLANE_ANGLE_UNIT ( ) SI_UNIT ( $, .RADIAN. ) );
#5124 = DIRECTION ( 'NONE',  ( 1.460819769243627131E-16, -1.000000000000000000, 0.000000000000000000 ) ) ;
#5125 = ORIENTED_EDGE ( 'NONE', *, *, #7329, .F. ) ;
#5126 = EDGE_CURVE ( 'NONE', #11114, #3954, #8062, .T. ) ;
#5127 = CIRCLE ( 'NONE', #13220, 2.649999999999985700 ) ;
#5128 = VERTEX_POINT ( 'NONE', #4685 ) ;
#5129 = DIRECTION ( 'NONE',  ( 0.000000000000000000, 0.000000000000000000, -1.000000000000000000 ) ) ;
#5130 = AXIS2_PLACEMENT_3D ( 'NONE', #8610, #8458, #681 ) ;
#5131 = VERTEX_POINT ( 'NONE', #5836 ) ;
#5132 = CARTESIAN_POINT ( 'NONE',  ( 229.9999999999999716, -85.00000000000007105, 190.0000000000000000 ) ) ;
#5133 = DIRECTION ( 'NONE',  ( -0.000000000000000000, 1.000000000000000000, -0.000000000000000000 ) ) ;
#5134 = CARTESIAN_POINT ( 'NONE',  ( -30.00000000000002842, -225.0000000000000000, 190.0000000000000000 ) ) ;
#5135 = EDGE_LOOP ( 'NONE', ( #13233, #9452 ) ) ;
#5136 = VECTOR ( 'NONE', #13013, 1000.000000000000114 ) ;
#5137 = CARTESIAN_POINT ( 'NONE',  ( 17.00000000000000000, 2.055000000000000160, 0.000000000000000000 ) ) ;
#5138 = LINE ( 'NONE', #4038, #660 ) ;
#5139 = DIRECTION ( 'NONE',  ( 0.000000000000000000, 0.000000000000000000, 1.000000000000000000 ) ) ;
#5140 = AXIS2_PLACEMENT_3D ( 'NONE', #87, #10058, #13314 ) ;
#5141 = DIRECTION ( 'NONE',  ( -1.000000000000000000, 0.000000000000000000, 0.000000000000000000 ) ) ;
#5142 = ORIENTED_EDGE ( 'NONE', *, *, #9370, .F. ) ;
#5143 = VECTOR ( 'NONE', #7911, 1000.000000000000000 ) ;
#5144 = EDGE_LOOP ( 'NONE', ( #847, #8562, #12265, #12251 ) ) ;
#5145 = DIRECTION ( 'NONE',  ( -0.000000000000000000, -0.000000000000000000, 1.000000000000000000 ) ) ;
#5146 = CARTESIAN_POINT ( 'NONE',  ( 469.9999999999998863, -225.0000000000000000, -190.0000000000000000 ) ) ;
#5147 = EDGE_CURVE ( 'NONE', #13924, #1600, #7161, .T. ) ;
#5148 = VECTOR ( 'NONE', #2286, 1000.000000000000000 ) ;
#5149 = EDGE_LOOP ( 'NONE', ( #860, #14067, #6468 ) ) ;
#5150 = CARTESIAN_POINT ( 'NONE',  ( 2.740000000000000213, -0.5149999999999973488, -0.6774776749089248540 ) ) ;
#5151 = PRESENTATION_LAYER_ASSIGNMENT (  '', '', ( #10937 ) ) ;
#5152 = DIRECTION ( 'NONE',  ( -1.000000000000000000, -0.000000000000000000, -0.000000000000000000 ) ) ;
#5153 = DIRECTION ( 'NONE',  ( -0.5000000000000051070, 1.060575238724903217E-16, -0.8660254037844355990 ) ) ;
#5154 = FACE_BOUND ( 'NONE', #13746, .T. ) ;
#5155 = CARTESIAN_POINT ( 'NONE',  ( 140.0000000000000000, -75.00000000000008527, -186.2999999999999829 ) ) ;
#5156 = VECTOR ( 'NONE', #7277, 1000.000000000000000 ) ;
#5157 = ORIENTED_EDGE ( 'NONE', *, *, #12073, .T. ) ;
#5158 = DIRECTION ( 'NONE',  ( -1.000000000000000000, 0.000000000000000000, 0.000000000000000000 ) ) ;
#5159 = AXIS2_PLACEMENT_3D ( 'NONE', #11509, #12524, #12661 ) ;
#5160 = ORIENTED_EDGE ( 'NONE', *, *, #7549, .F. ) ;
#5161 = VECTOR ( 'NONE', #12929, 1000.000000000000000 ) ;
#5162 = DIRECTION ( 'NONE',  ( -0.000000000000000000, 0.000000000000000000, -1.000000000000000000 ) ) ;
#5163 = DIRECTION ( 'NONE',  ( -1.000000000000000000, -0.000000000000000000, -0.000000000000000000 ) ) ;
#5164 = EDGE_CURVE ( 'NONE', #3114, #9120, #1815, .T. ) ;
#5165 = PRODUCT_DEFINITION ( 'UNKNOWN', '', #5409, #9636 ) ;
#5166 = ORIENTED_EDGE ( 'NONE', *, *, #2777, .T. ) ;
#5167 = CARTESIAN_POINT ( 'NONE',  ( -20.63749999999999929, 0.000000000000000000, -11.05000000000000071 ) ) ;
#5168 = ORIENTED_EDGE ( 'NONE', *, *, #1169, .T. ) ;
#5169 = LINE ( 'NONE', #12913, #2225 ) ;
#5170 = DIRECTION ( 'NONE',  ( -1.000000000000000000, -0.000000000000000000, -0.000000000000000000 ) ) ;
#5171 = ORIENTED_EDGE ( 'NONE', *, *, #7820, .F. ) ;
#5172 = SURFACE_SIDE_STYLE ('',( #11975 ) ) ;
#5173 = EDGE_CURVE ( 'NONE', #2036, #5508, #5906, .T. ) ;
#5174 = DIRECTION ( 'NONE',  ( -1.000000000000000000, -0.000000000000000000, -0.000000000000000000 ) ) ;
#5175 = CYLINDRICAL_SURFACE ( 'NONE', #13803, 2.500000000000002220 ) ;
#5176 =( NAMED_UNIT ( * ) PLANE_ANGLE_UNIT ( ) SI_UNIT ( $, .RADIAN. ) );
#5177 = CIRCLE ( 'NONE', #7011, 7.864440107515430434 ) ;
#5178 = DIRECTION ( 'NONE',  ( -1.000000000000000000, -0.000000000000000000, -0.000000000000000000 ) ) ;
#5179 = EDGE_CURVE ( 'NONE', #4205, #1111, #9023, .T. ) ;
#5180 = EDGE_CURVE ( 'NONE', #678, #2602, #8090, .T. ) ;
#5181 = DIRECTION ( 'NONE',  ( -1.000000000000000000, 0.000000000000000000, 0.000000000000000000 ) ) ;
#5182 = ORIENTED_EDGE ( 'NONE', *, *, #2089, .F. ) ;
#5183 = VERTEX_POINT ( 'NONE', #12368 ) ;
#5184 = ORIENTED_EDGE ( 'NONE', *, *, #2140, .T. ) ;
#5185 = EDGE_LOOP ( 'NONE', ( #9594, #347 ) ) ;
#5186 = CARTESIAN_POINT ( 'NONE',  ( 219.9999999999999716, -25.00000000000000000, -225.1500000000000625 ) ) ;
#5187 = EDGE_CURVE ( 'NONE', #3312, #8807, #12729, .T. ) ;
#5188 = ORIENTED_EDGE ( 'NONE', *, *, #1501, .F. ) ;
#5189 = CARTESIAN_POINT ( 'NONE',  ( 2.500000000000000000, -1.178949249685214307, 2.042000000000001592 ) ) ;
#5190 = ORIENTED_EDGE ( 'NONE', *, *, #8080, .T. ) ;
#5191 = LINE ( 'NONE', #14089, #1775 ) ;
#5192 = EDGE_LOOP ( 'NONE', ( #268, #7880, #13626, #4542 ) ) ;
#5193 = CARTESIAN_POINT ( 'NONE',  ( 299.9999999999999432, -95.00000000000008527, -169.9999999999999716 ) ) ;
#5194 = UNCERTAINTY_MEASURE_WITH_UNIT (LENGTH_MEASURE( 1.000000000000000082E-05 ), #5818, 'distance_accuracy_value', 'NONE');
#5195 = FACE_OUTER_BOUND ( 'NONE', #13267, .T. ) ;
#5196 = DIRECTION ( 'NONE',  ( 1.000000000000000000, 0.000000000000000000, 0.000000000000000000 ) ) ;
#5197 = CARTESIAN_POINT ( 'NONE',  ( 269.0000000000000000, 8.660254037844390851, 200.0000000000000000 ) ) ;
#5198 = EDGE_CURVE ( 'NONE', #9987, #7747, #10956, .T. ) ;
#5199 = DIRECTION ( 'NONE',  ( 0.000000000000000000, 0.000000000000000000, 1.000000000000000000 ) ) ;
#5200 = ORIENTED_EDGE ( 'NONE', *, *, #5492, .F. ) ;
#5201 = EDGE_LOOP ( 'NONE', ( #6609, #3542 ) ) ;
#5202 = EDGE_CURVE ( 'NONE', #417, #1810, #13195, .T. ) ;
#5203 = DIRECTION ( 'NONE',  ( 0.000000000000000000, -1.000000000000000000, 0.000000000000000000 ) ) ;
#5204 = CARTESIAN_POINT ( 'NONE',  ( 16.55500000000001393, 0.000000000000000000, 0.000000000000000000 ) ) ;
#5205 = CARTESIAN_POINT ( 'NONE',  ( 219.9999999999999716, -15.00000000000000000, 225.1500000000000625 ) ) ;
#5206 = ORIENTED_EDGE ( 'NONE', *, *, #34, .T. ) ;
#5207 = CARTESIAN_POINT ( 'NONE',  ( -134.9999999999999716, 45.00000000000001421, 30.00000000000000000 ) ) ;
#5208 = LINE ( 'NONE', #9554, #183 ) ;
#5209 = DIRECTION ( 'NONE',  ( 1.000000000000000000, 0.000000000000000000, 0.000000000000000000 ) ) ;
#5210 = CARTESIAN_POINT ( 'NONE',  ( 2.500000000000000000, 1.178949249685218525, 2.041999999999999371 ) ) ;
#5211 = ORIENTED_EDGE ( 'NONE', *, *, #9330, .T. ) ;
#5212 = ORIENTED_EDGE ( 'NONE', *, *, #9123, .F. ) ;
#5213 = CARTESIAN_POINT ( 'NONE',  ( 211.3397459621556038, -80.00000000000007105, 55.00000000000002132 ) ) ;
#5214 = PRODUCT_DEFINITION_SHAPE ( 'NONE', 'NONE',  #14357 ) ;
#5215 = CARTESIAN_POINT ( 'NONE',  ( -144.9999999999999432, -65.00000000000008527, 30.00000000000000000 ) ) ;
#5216 = ADVANCED_FACE ( 'NONE', ( #3592 ), #4609, .T. ) ;
#5217 = ORIENTED_EDGE ( 'NONE', *, *, #7973, .F. ) ;
#5218 = CARTESIAN_POINT ( 'NONE',  ( -137.6499999999999773, 45.00000000000001421, 40.00000000000000000 ) ) ;
#5219 = DIRECTION ( 'NONE',  ( 0.000000000000000000, 0.000000000000000000, -1.000000000000000000 ) ) ;
#5220 = CARTESIAN_POINT ( 'NONE',  ( 4.211399257449709665, -2.459727064652517114, -3.751161691472417736 ) ) ;
#5221 = DIRECTION ( 'NONE',  ( 0.000000000000000000, 1.000000000000000000, -1.224646799147353207E-16 ) ) ;
#5222 = DIRECTION ( 'NONE',  ( 1.000000000000000000, 0.000000000000000000, 0.000000000000000000 ) ) ;
#5223 = CLOSED_SHELL ( 'NONE', ( #9787, #12921, #10489, #9524, #10020, #6916, #3372, #4392, #6411, #1502, #1664, #8664 ) ) ;
#5224 = ITEM_DEFINED_TRANSFORMATION ( 'NONE', 'NONE', #5840,  #14039 ) ;
#5225 = ORIENTED_EDGE ( 'NONE', *, *, #12168, .F. ) ;
#5226 = DIRECTION ( 'NONE',  ( 0.000000000000000000, 0.000000000000000000, -1.000000000000000000 ) ) ;
#5227 = ORIENTED_EDGE ( 'NONE', *, *, #7894, .F. ) ;
#5228 = CARTESIAN_POINT ( 'NONE',  ( -314.9999999999999432, 55.00000000000001421, 30.00000000000000000 ) ) ;
#5229 = CYLINDRICAL_SURFACE ( 'NONE', #2318, 2.649999999999985700 ) ;
#5230 = VERTEX_POINT ( 'NONE', #3731 ) ;
#5231 = CARTESIAN_POINT ( 'NONE',  ( 134.9999999999999432, -56.99999999999997158, 10.00000000000000178 ) ) ;
#5232 = ORIENTED_EDGE ( 'NONE', *, *, #12814, .T. ) ;
#5233 = DIRECTION ( 'NONE',  ( -1.000000000000000000, 2.312964634635743450E-16, 0.000000000000000000 ) ) ;
#5234 = CARTESIAN_POINT ( 'NONE',  ( 0.000000000000000000, 0.000000000000000000, 0.000000000000000000 ) ) ;
#5235 = ORIENTED_EDGE ( 'NONE', *, *, #9106, .F. ) ;
#5236 = FACE_OUTER_BOUND ( 'NONE', #5976, .T. ) ;
#5237 = DIRECTION ( 'NONE',  ( 0.000000000000000000, 0.000000000000000000, -1.000000000000000000 ) ) ;
#5238 = SURFACE_STYLE_FILL_AREA ( #11837 ) ;
#5239 = EDGE_CURVE ( 'NONE', #1677, #12041, #9027, .T. ) ;
#5240 = ITEM_DEFINED_TRANSFORMATION ( 'NONE', 'NONE', #3530,  #14039 ) ;
#5241 = CARTESIAN_POINT ( 'NONE',  ( -145.0000000000000284, -75.00000000000008527, 40.00000000000000000 ) ) ;
#5242 = VECTOR ( 'NONE', #3708, 1000.000000000000000 ) ;
#5243 = EDGE_CURVE ( 'NONE', #12400, #13943, #10657, .T. ) ;
#5244 = ORIENTED_EDGE ( 'NONE', *, *, #6939, .T. ) ;
#5245 = AXIS2_PLACEMENT_3D ( 'NONE', #2233, #1271, #9118 ) ;
#5246 = ORIENTED_EDGE ( 'NONE', *, *, #2606, .T. ) ;
#5247 = FACE_OUTER_BOUND ( 'NONE', #480, .T. ) ;
#5248 = ORIENTED_EDGE ( 'NONE', *, *, #2655, .F. ) ;
#5249 = FACE_OUTER_BOUND ( 'NONE', #3934, .T. ) ;
#5250 = EDGE_LOOP ( 'NONE', ( #11925, #12792, #12559, #13482 ) ) ;
#5251 = EDGE_LOOP ( 'NONE', ( #5575, #14173 ) ) ;
#5252 = DIRECTION ( 'NONE',  ( -0.000000000000000000, 1.000000000000000000, 1.224646799147353207E-16 ) ) ;
#5253 = VERTEX_POINT ( 'NONE', #11216 ) ;
#5254 = LINE ( 'NONE', #2047, #2917 ) ;
#5255 = CIRCLE ( 'NONE', #9171, 2.649999999999985700 ) ;
#5256 = DIRECTION ( 'NONE',  ( -0.000000000000000000, 1.000000000000000000, 0.000000000000000000 ) ) ;
#5257 = CARTESIAN_POINT ( 'NONE',  ( 53.33333333333330017, -20.00000000000000000, 219.8500000000001080 ) ) ;
#5258 = ADVANCED_BREP_SHAPE_REPRESENTATION ( '', ( #13412, #14039 ), #1410 ) ;
#5259 = AXIS2_PLACEMENT_3D ( 'NONE', #1887, #10749, #775 ) ;
#5260 = DIRECTION ( 'NONE',  ( 0.000000000000000000, -1.000000000000000000, 0.000000000000000000 ) ) ;
#5261 = ADVANCED_FACE ( 'NONE', ( #10117 ), #153, .F. ) ;
#5262 = ADVANCED_FACE ( 'NONE', ( #12802 ), #1846, .T. ) ;
#5263 = FACE_OUTER_BOUND ( 'NONE', #2326, .T. ) ;
#5264 = VECTOR ( 'NONE', #6604, 1000.000000000000000 ) ;
#5265 = ORIENTED_EDGE ( 'NONE', *, *, #800, .T. ) ;
#5266 = AXIS2_PLACEMENT_3D ( 'NONE', #14194, #8616, #5219 ) ;
#5267 = ORIENTED_EDGE ( 'NONE', *, *, #9608, .T. ) ;
#5268 = CIRCLE ( 'NONE', #13351, 2.500000000000000444 ) ;
#5269 = LINE ( 'NONE', #10634, #6561 ) ;
#5270 = ORIENTED_EDGE ( 'NONE', *, *, #13523, .F. ) ;
#5271 = CARTESIAN_POINT ( 'NONE',  ( 2.000000000000001776, 0.000000000000000000, -13.29999999999999893 ) ) ;
#5272 = DIRECTION ( 'NONE',  ( 0.000000000000000000, 0.000000000000000000, -1.000000000000000000 ) ) ;
#5273 = EDGE_CURVE ( 'NONE', #3734, #6981, #3015, .T. ) ;
#5274 = ADVANCED_FACE ( 'NONE', ( #9542 ), #6266, .T. ) ;
#5275 = DIRECTION ( 'NONE',  ( 1.000000000000000000, 0.000000000000000000, 0.000000000000000000 ) ) ;
#5276 = CIRCLE ( 'NONE', #2717, 4.000000000000000000 ) ;
#5277 = ORIENTED_EDGE ( 'NONE', *, *, #802, .F. ) ;
#5278 = EDGE_CURVE ( 'NONE', #13138, #13081, #11710, .T. ) ;
#5279 = COLOUR_RGB ( '',0.8941176470588234615, 0.8941176470588234615, 0.8941176470588234615 ) ;
#5280 = CARTESIAN_POINT ( 'NONE',  ( 2.500000000000000000, 1.178949249685213863, -2.042000000000001148 ) ) ;
#5281 = EDGE_CURVE ( 'NONE', #12345, #11223, #11094, .T. ) ;
#5282 = TOROIDAL_SURFACE ( 'NONE', #10120, 2.700000000000001066, 0.2000000000000000111 ) ;
#5283 = CARTESIAN_POINT ( 'NONE',  ( 201.0000000000000000, -85.00000000000007105, 190.0000000000000000 ) ) ;
#5284 = DIRECTION ( 'NONE',  ( 6.123233995736766036E-17, 0.000000000000000000, -1.000000000000000000 ) ) ;
#5285 = CIRCLE ( 'NONE', #13365, 11.05000000000000071 ) ;
#5286 = DIRECTION ( 'NONE',  ( 0.000000000000000000, 0.000000000000000000, 1.000000000000000000 ) ) ;
#5287 = ORIENTED_EDGE ( 'NONE', *, *, #12821, .F. ) ;
#5288 = TOROIDAL_SURFACE ( 'NONE', #8026, 2.700000000000001066, 0.2000000000000000111 ) ;
#5289 = VERTEX_POINT ( 'NONE', #10774 ) ;
#5290 = CARTESIAN_POINT ( 'NONE',  ( -31.74999999999995737, 0.000000000000000000, 0.000000000000000000 ) ) ;
#5291 = AXIS2_PLACEMENT_3D ( 'NONE', #6950, #1279, #3419 ) ;
#5292 = LINE ( 'NONE', #7301, #9288 ) ;
#5293 = AXIS2_PLACEMENT_3D ( 'NONE', #2985, #4139, #6239 ) ;
#5294 = ORIENTED_EDGE ( 'NONE', *, *, #5147, .F. ) ;
#5295 = CARTESIAN_POINT ( 'NONE',  ( 5.200000000000002842, 0.000000000000000000, 0.000000000000000000 ) ) ;
#5296 = CYLINDRICAL_SURFACE ( 'NONE', #6955, 12.00000000000000000 ) ;
#5297 = PLANE ( 'NONE',  #7148 ) ;
#5298 = SHAPE_REPRESENTATION_RELATIONSHIP ( 'NONE' , 'NONE' ,  #10314, #1248 ) ;
#5299 = AXIS2_PLACEMENT_3D ( 'NONE', #1624, #8084, #370 ) ;
#5300 = ADVANCED_FACE ( 'NONE', ( #804 ), #2721, .F. ) ;
#5301 = VERTEX_POINT ( 'NONE', #9612 ) ;
#5302 = DIRECTION ( 'NONE',  ( -0.000000000000000000, -0.000000000000000000, -1.000000000000000000 ) ) ;
#5303 = EDGE_LOOP ( 'NONE', ( #9674, #7778 ) ) ;
#5304 = CARTESIAN_POINT ( 'NONE',  ( -5.384454397937118664, 6.594054843588581554E-16, -4.484454397937119197 ) ) ;
#5305 = CARTESIAN_POINT ( 'NONE',  ( 2.740000000000000213, 0.6774776749089226335, -0.5150000000000000133 ) ) ;
#5306 = VERTEX_POINT ( 'NONE', #2794 ) ;
#5307 = LINE ( 'NONE', #9727, #4347 ) ;
#5308 = ORIENTED_EDGE ( 'NONE', *, *, #2479, .F. ) ;
#5309 = CARTESIAN_POINT ( 'NONE',  ( 239.1499999999999204, -85.00000000000007105, 55.00000000000001421 ) ) ;
#5310 = CARTESIAN_POINT ( 'NONE',  ( -4.000000000000000000, 0.3987449864459974846, -0.01220643443059782861 ) ) ;
#5311 = EDGE_LOOP ( 'NONE', ( #13955, #7155, #9604, #3995, #14191, #6739 ) ) ;
#5312 = VECTOR ( 'NONE', #3557, 999.9999999999998863 ) ;
#5313 = CARTESIAN_POINT ( 'NONE',  ( 2.740000000000000213, 0.9838866223910003317, 0.5149999999999999023 ) ) ;
#5314 = DIRECTION ( 'NONE',  ( -0.000000000000000000, -0.000000000000000000, 1.000000000000000000 ) ) ;
#5315 = CARTESIAN_POINT ( 'NONE',  ( -4.000000000000000000, 0.8730739991738342143, -3.223134629628428893 ) ) ;
#5316 = VERTEX_POINT ( 'NONE', #14018 ) ;
#5317 = ORIENTED_EDGE ( 'NONE', *, *, #4278, .T. ) ;
#5318 = CARTESIAN_POINT ( 'NONE',  ( -4.999999999999997335, -8.660254037844389075, 200.0000000000000000 ) ) ;
#5319 = VERTEX_POINT ( 'NONE', #581 ) ;
#5320 = DIRECTION ( 'NONE',  ( -0.000000000000000000, 1.000000000000000000, -0.000000000000000000 ) ) ;
#5321 = AXIS2_PLACEMENT_3D ( 'NONE', #3402, #1120, #5567 ) ;
#5322 = VERTEX_POINT ( 'NONE', #8294 ) ;
#5323 = ORIENTED_EDGE ( 'NONE', *, *, #11382, .T. ) ;
#5324 = CARTESIAN_POINT ( 'NONE',  ( 136.6666666666666288, -25.00000000000000000, -219.8500000000001080 ) ) ;
#5325 = VERTEX_POINT ( 'NONE', #6124 ) ;
#5326 = ADVANCED_FACE ( 'NONE', ( #2936 ), #3803, .F. ) ;
#5327 = DIRECTION ( 'NONE',  ( -0.000000000000000000, -0.000000000000000000, 1.000000000000000000 ) ) ;
#5328 = LINE ( 'NONE', #10910, #9680 ) ;
#5329 = DIRECTION ( 'NONE',  ( 1.000000000000000000, 0.000000000000000000, 0.000000000000000000 ) ) ;
#5330 = CIRCLE ( 'NONE', #13417, 2.649999999999985700 ) ;
#5331 = CARTESIAN_POINT ( 'NONE',  ( -5.000000000000000888, 0.000000000000000000, -200.0000000000000000 ) ) ;
#5332 = SHAPE_REPRESENTATION ( 'roller axis', ( #14039 ), #5930 ) ;
#5333 = EDGE_LOOP ( 'NONE', ( #7625, #9298 ) ) ;
#5334 = AXIS2_PLACEMENT_3D ( 'NONE', #9576, #12022, #11949 ) ;
#5335 = VERTEX_POINT ( 'NONE', #13951 ) ;
#5336 = CARTESIAN_POINT ( 'NONE',  ( 386.6666666666666288, -20.00000000000000000, 219.8500000000001080 ) ) ;
#5337 = VERTEX_POINT ( 'NONE', #10479 ) ;
#5338 = DIRECTION ( 'NONE',  ( 0.000000000000000000, 0.000000000000000000, -1.000000000000000000 ) ) ;
#5339 = ADVANCED_FACE ( 'NONE', ( #13877 ), #7428, .F. ) ;
#5340 = DIRECTION ( 'NONE',  ( -1.000000000000000000, 0.000000000000000000, -0.000000000000000000 ) ) ;
#5341 = FACE_OUTER_BOUND ( 'NONE', #1001, .T. ) ;
#5342 = VECTOR ( 'NONE', #4993, 1000.000000000000000 ) ;
#5343 = EDGE_LOOP ( 'NONE', ( #3847, #1207 ) ) ;
#5344 = AXIS2_PLACEMENT_3D ( 'NONE', #1929, #13893, #1857 ) ;
#5345 = VECTOR ( 'NONE', #1818, 1000.000000000000000 ) ;
#5346 = DIRECTION ( 'NONE',  ( 0.000000000000000000, 0.000000000000000000, 1.000000000000000000 ) ) ;
#5347 = CARTESIAN_POINT ( 'NONE',  ( 0.06760930072668806801, -4.837354856632045452E-15, 0.000000000000000000 ) ) ;
#5348 = CARTESIAN_POINT ( 'NONE',  ( 305.0000000000000000, -36.99999999999997868, -154.9999999999999716 ) ) ;
#5349 = CARTESIAN_POINT ( 'NONE',  ( 219.9999999999999716, -85.00000000000007105, 170.0000000000000000 ) ) ;
#5350 = ADVANCED_FACE ( 'NONE', ( #5263 ), #1837, .T. ) ;
#5351 = EDGE_CURVE ( 'NONE', #11341, #5839, #10631, .T. ) ;
#5352 = EDGE_LOOP ( 'NONE', ( #2712, #8869 ) ) ;
#5353 = AXIS2_PLACEMENT_3D ( 'NONE', #907, #11823, #13051 ) ;
#5354 = ADVANCED_FACE ( 'NONE', ( #10703 ), #12942, .T. ) ;
#5355 = ORIENTED_EDGE ( 'NONE', *, *, #164, .T. ) ;
#5356 = DIRECTION ( 'NONE',  ( 0.8949343913984143528, 0.4461977533474922875, 0.000000000000000000 ) ) ;
#5357 = DIRECTION ( 'NONE',  ( 0.000000000000000000, 0.000000000000000000, 1.000000000000000000 ) ) ;
#5358 = VERTEX_POINT ( 'NONE', #734 ) ;
#5359 = CARTESIAN_POINT ( 'NONE',  ( 0.000000000000000000, 0.000000000000000000, 4.000000000000000000 ) ) ;
#5360 = VECTOR ( 'NONE', #6855, 1000.000000000000000 ) ;
#5361 = FACE_OUTER_BOUND ( 'NONE', #2024, .T. ) ;
#5362 = LINE ( 'NONE', #10736, #3463 ) ;
#5363 = SURFACE_STYLE_FILL_AREA ( #2011 ) ;
#5364 = APPLICATION_CONTEXT ( 'automotive_design' ) ;
#5365 = VECTOR ( 'NONE', #8822, 1000.000000000000000 ) ;
#5366 = EDGE_CURVE ( 'NONE', #5028, #417, #3877, .T. ) ;
#5367 = ORIENTED_EDGE ( 'NONE', *, *, #1576, .F. ) ;
#5368 = DIRECTION ( 'NONE',  ( -0.000000000000000000, -1.000000000000000000, -0.000000000000000000 ) ) ;
#5369 = VERTEX_POINT ( 'NONE', #8514 ) ;
#5370 = LINE ( 'NONE', #5228, #12789 ) ;
#5371 = CARTESIAN_POINT ( 'NONE',  ( 214.9999999999999716, -85.00000000000007105, 50.00000000000001421 ) ) ;
#5372 = AXIS2_PLACEMENT_3D ( 'NONE', #9852, #8763, #8383 ) ;
#5373 = ORIENTED_EDGE ( 'NONE', *, *, #3151, .F. ) ;
#5374 = EDGE_LOOP ( 'NONE', ( #664, #6817 ) ) ;
#5375 = PLANE ( 'NONE',  #5926 ) ;
#5376 = VERTEX_POINT ( 'NONE', #12940 ) ;
#5377 = DIRECTION ( 'NONE',  ( 1.000000000000000000, 0.000000000000000000, 0.000000000000000000 ) ) ;
#5378 = CARTESIAN_POINT ( 'NONE',  ( -30.00000000000002842, -25.00000000000000000, 250.0000000000000000 ) ) ;
#5379 = FILL_AREA_STYLE ('',( #14215 ) ) ;
#5380 = VECTOR ( 'NONE', #5834, 1000.000000000000000 ) ;
#5381 = AXIS2_PLACEMENT_3D ( 'NONE', #10741, #4136, #13190 ) ;
#5382 = CARTESIAN_POINT ( 'NONE',  ( 3.699999999999998401, 5.817072295949927426E-16, -4.750000000000000000 ) ) ;
#5383 = CARTESIAN_POINT ( 'NONE',  ( -1.655952806101422814, 3.662737355149034979, -7.623296525288699970E-18 ) ) ;
#5384 = VERTEX_POINT ( 'NONE', #14233 ) ;
#5385 = VECTOR ( 'NONE', #571, 1000.000000000000000 ) ;
#5386 = VERTEX_POINT ( 'NONE', #8587 ) ;
#5387 = DIRECTION ( 'NONE',  ( -0.000000000000000000, -0.000000000000000000, 1.000000000000000000 ) ) ;
#5388 = VERTEX_POINT ( 'NONE', #7498 ) ;
#5389 = DIRECTION ( 'NONE',  ( -0.000000000000000000, -0.000000000000000000, 1.000000000000000000 ) ) ;
#5390 = UNCERTAINTY_MEASURE_WITH_UNIT (LENGTH_MEASURE( 1.000000000000000082E-05 ), #2971, 'distance_accuracy_value', 'NONE');
#5391 = ORIENTED_EDGE ( 'NONE', *, *, #4327, .F. ) ;
#5392 = AXIS2_PLACEMENT_3D ( 'NONE', #14026, #4102, #442 ) ;
#5393 = ORIENTED_EDGE ( 'NONE', *, *, #10743, .T. ) ;
#5394 = PLANE ( 'NONE',  #10352 ) ;
#5395 = EDGE_LOOP ( 'NONE', ( #5232, #11828, #7892, #2601 ) ) ;
#5396 = CARTESIAN_POINT ( 'NONE',  ( 303.3333333333333144, -20.00000000000000000, 222.5000000000000853 ) ) ;
#5397 = AXIS2_PLACEMENT_3D ( 'NONE', #960, #4260, #12415 ) ;
#5398 = CARTESIAN_POINT ( 'NONE',  ( 4.024499207728848837, 2.323545700935681246, -3.572172305156870564 ) ) ;
#5399 = STYLED_ITEM ( 'NONE', ( #204 ), #7317 ) ;
#5400 = CARTESIAN_POINT ( 'NONE',  ( 434.9999999999999432, 8.660254037844390851, 200.0000000000000000 ) ) ;
#5401 = EDGE_CURVE ( 'NONE', #2336, #7714, #4343, .T. ) ;
#5402 = AXIS2_PLACEMENT_3D ( 'NONE', #9214, #5733, #10372 ) ;
#5403 = DIRECTION ( 'NONE',  ( 0.000000000000000000, -0.5000000000000009992, -0.8660254037844380415 ) ) ;
#5404 = DIRECTION ( 'NONE',  ( 0.000000000000000000, 1.000000000000000000, 0.000000000000000000 ) ) ;
#5405 = CIRCLE ( 'NONE', #10966, 0.2000000000000000944 ) ;
#5406 = ORIENTED_EDGE ( 'NONE', *, *, #2870, .F. ) ;
#5407 = ADVANCED_FACE ( 'NONE', ( #8731 ), #11934, .F. ) ;
#5408 = VERTEX_POINT ( 'NONE', #4389 ) ;
#5409 = PRODUCT_DEFINITION_FORMATION_WITH_SPECIFIED_SOURCE ( 'ANY', '', #3459, .NOT_KNOWN. ) ;
#5410 = CARTESIAN_POINT ( 'NONE',  ( 2.500000000000000000, -2.357898499370432166, 3.035766082959412415E-15 ) ) ;
#5411 = ORIENTED_EDGE ( 'NONE', *, *, #12085, .T. ) ;
#5412 = DIRECTION ( 'NONE',  ( -0.000000000000000000, 1.000000000000000000, -0.000000000000000000 ) ) ;
#5413 = CARTESIAN_POINT ( 'NONE',  ( 1.747541505913279281, -3.837784562140273081, -3.503702292528912299 ) ) ;
#5414 = ORIENTED_EDGE ( 'NONE', *, *, #6068, .F. ) ;
#5415 = CARTESIAN_POINT ( 'NONE',  ( 134.9999999999999716, 45.00000000000001421, 10.00000000000000000 ) ) ;
#5416 = DIRECTION ( 'NONE',  ( -1.000000000000000000, -0.000000000000000000, -0.000000000000000000 ) ) ;
#5417 = DIRECTION ( 'NONE',  ( -6.123233995736766036E-17, 0.000000000000000000, -1.000000000000000000 ) ) ;
#5418 = PLANE ( 'NONE',  #4759 ) ;
#5419 = ADVANCED_FACE ( 'NONE', ( #1981, #2199, #4311 ), #13293, .F. ) ;
#5420 = ORIENTED_EDGE ( 'NONE', *, *, #8564, .F. ) ;
#5421 = EDGE_CURVE ( 'NONE', #13943, #12400, #6877, .T. ) ;
#5422 = EDGE_LOOP ( 'NONE', ( #7007, #40, #5645, #6400 ) ) ;
#5423 = DIRECTION ( 'NONE',  ( 0.000000000000000000, 0.5000000000000011102, 0.8660254037844380415 ) ) ;
#5424 = LINE ( 'NONE', #9846, #3510 ) ;
#5425 = ORIENTED_EDGE ( 'NONE', *, *, #7150, .T. ) ;
#5426 = PLANE ( 'NONE',  #2462 ) ;
#5427 = EDGE_CURVE ( 'NONE', #4302, #7253, #12074, .T. ) ;
#5428 = CYLINDRICAL_SURFACE ( 'NONE', #885, 12.77499999999999858 ) ;
#5429 = DIRECTION ( 'NONE',  ( 0.000000000000000000, 0.000000000000000000, 1.000000000000000000 ) ) ;
#5430 = ADVANCED_FACE ( 'NONE', ( #3162 ), #6626, .F. ) ;
#5431 = EDGE_LOOP ( 'NONE', ( #2350, #401, #294, #5666, #13324 ) ) ;
#5432 = DIRECTION ( 'NONE',  ( 0.000000000000000000, 0.000000000000000000, -1.000000000000000000 ) ) ;
#5433 = ORIENTED_EDGE ( 'NONE', *, *, #2279, .T. ) ;
#5434 = CARTESIAN_POINT ( 'NONE',  ( -0.1404048886732797152, -4.699864953788083888, -3.686887068327043160 ) ) ;
#5435 = CARTESIAN_POINT ( 'NONE',  ( 140.0000000000000000, -75.00000000000008527, -190.0000000000000000 ) ) ;
#5436 = ORIENTED_EDGE ( 'NONE', *, *, #1221, .F. ) ;
#5437 = VERTEX_POINT ( 'NONE', #6560 ) ;
#5438 = DIRECTION ( 'NONE',  ( 1.000000000000000000, 0.000000000000000000, 0.000000000000000000 ) ) ;
#5439 = ADVANCED_FACE ( 'NONE', ( #3305 ), #7588, .T. ) ;
#5440 = PRODUCT_DEFINITION_SHAPE ( 'NONE', 'NONE',  #14332 ) ;
#5441 = DIRECTION ( 'NONE',  ( 0.000000000000000000, -1.000000000000000000, 0.000000000000000000 ) ) ;
#5442 = EDGE_CURVE ( 'NONE', #7879, #8136, #2274, .T. ) ;
#5443 = CARTESIAN_POINT ( 'NONE',  ( 134.9999999999999432, -36.99999999999997868, -169.9999999999999716 ) ) ;
#5444 = CARTESIAN_POINT ( 'NONE',  ( 302.4999999999999432, 45.00000000000001421, 0.000000000000000000 ) ) ;
#5445 = DIRECTION ( 'NONE',  ( 0.000000000000000000, -0.5000000000000011102, -0.8660254037844379305 ) ) ;
#5446 = FACE_BOUND ( 'NONE', #14080, .T. ) ;
#5447 = EDGE_CURVE ( 'NONE', #722, #4527, #5541, .T. ) ;
#5448 = CARTESIAN_POINT ( 'NONE',  ( 319.9999999999999432, -20.00000000000000000, -19.99999999999998934 ) ) ;
#5449 = ORIENTED_EDGE ( 'NONE', *, *, #11834, .F. ) ;
#5450 = ORIENTED_EDGE ( 'NONE', *, *, #13006, .F. ) ;
#5451 = DIRECTION ( 'NONE',  ( -1.000000000000000000, -0.000000000000000000, -0.000000000000000000 ) ) ;
#5452 = VECTOR ( 'NONE', #2330, 1000.000000000000000 ) ;
#5453 = ORIENTED_EDGE ( 'NONE', *, *, #2224, .T. ) ;
#5454 = LINE ( 'NONE', #5599, #10948 ) ;
#5455 = EDGE_LOOP ( 'NONE', ( #1759, #5168, #3063 ) ) ;
#5456 = VERTEX_POINT ( 'NONE', #13014 ) ;
#5457 = LINE ( 'NONE', #11049, #8737 ) ;
#5458 = ORIENTED_EDGE ( 'NONE', *, *, #14291, .T. ) ;
#5459 = DIRECTION ( 'NONE',  ( -1.000000000000000000, -0.000000000000000000, -0.000000000000000000 ) ) ;
#5460 = CARTESIAN_POINT ( 'NONE',  ( 0.000000000000000000, 0.000000000000000000, 200.0000000000000000 ) ) ;
#5461 = CARTESIAN_POINT ( 'NONE',  ( 0.000000000000000000, 0.000000000000000000, 0.000000000000000000 ) ) ;
#5462 = CIRCLE ( 'NONE', #14022, 5.000000000000004441 ) ;
#5463 = LINE ( 'NONE', #4455, #11819 ) ;
#5464 = LINE ( 'NONE', #4244, #2487 ) ;
#5465 = ORIENTED_EDGE ( 'NONE', *, *, #6767, .T. ) ;
#5466 = ORIENTED_EDGE ( 'NONE', *, *, #4605, .F. ) ;
#5467 = EDGE_CURVE ( 'NONE', #791, #3217, #5464, .T. ) ;
#5468 = CARTESIAN_POINT ( 'NONE',  ( 197.5000000000000000, -80.00000000000007105, 50.00000000000001421 ) ) ;
#5469 = AXIS2_PLACEMENT_3D ( 'NONE', #11590, #3825, #2666 ) ;
#5470 = VERTEX_POINT ( 'NONE', #5614 ) ;
#5471 = DIRECTION ( 'NONE',  ( -0.000000000000000000, 0.000000000000000000, -1.000000000000000000 ) ) ;
#5472 = DIRECTION ( 'NONE',  ( 0.000000000000000000, 0.000000000000000000, -1.000000000000000000 ) ) ;
#5473 = AXIS2_PLACEMENT_3D ( 'NONE', #10605, #3927, #6243 ) ;
#5474 = CARTESIAN_POINT ( 'NONE',  ( 5.200000000000002842, 3.061616997868383634E-16, -2.500000000000000444 ) ) ;
#5475 = ORIENTED_EDGE ( 'NONE', *, *, #1609, .T. ) ;
#5476 = VECTOR ( 'NONE', #6072, 1000.000000000000000 ) ;
#5477 = DIRECTION ( 'NONE',  ( -0.000000000000000000, 1.000000000000000000, -0.000000000000000000 ) ) ;
#5478=STYLED_ITEM('',(#14417),#8659);
#5479 = VECTOR ( 'NONE', #10258, 1000.000000000000114 ) ;
#5480 = DIRECTION ( 'NONE',  ( -0.000000000000000000, -0.000000000000000000, -1.000000000000000000 ) ) ;
#5481 = DIRECTION ( 'NONE',  ( 0.000000000000000000, 0.000000000000000000, 1.000000000000000000 ) ) ;
#5482 = VECTOR ( 'NONE', #13650, 1000.000000000000000 ) ;
#5483 = ORIENTED_EDGE ( 'NONE', *, *, #2513, .T. ) ;
#5484 = EDGE_CURVE ( 'NONE', #9676, #5579, #5965, .T. ) ;
#5485 =( REPRESENTATION_RELATIONSHIP ('NONE','NONE', #11251, #13104 ) REPRESENTATION_RELATIONSHIP_WITH_TRANSFORMATION ( #9927 )SHAPE_REPRESENTATION_RELATIONSHIP( ) );
#5486 = DIRECTION ( 'NONE',  ( 0.000000000000000000, 3.656775105596099119E-15, -1.000000000000000000 ) ) ;
#5487 = AXIS2_PLACEMENT_3D ( 'NONE', #13439, #9021, #3520 ) ;
#5488 = DIRECTION ( 'NONE',  ( -1.000000000000000000, -0.000000000000000000, -0.000000000000000000 ) ) ;
#5489 = AXIS2_PLACEMENT_3D ( 'NONE', #8660, #9682, #1977 ) ;
#5490 = ORIENTED_EDGE ( 'NONE', *, *, #7636, .T. ) ;
#5492 = EDGE_CURVE ( 'NONE', #10676, #1275, #3430, .T. ) ;
#5491 = CARTESIAN_POINT ( 'NONE',  ( 142.6500000000000057, -95.00000000000008527, 169.9999999999999716 ) ) ;
#5493 = VECTOR ( 'NONE', #5601, 1000.000000000000000 ) ;
#5494 = AXIS2_PLACEMENT_3D ( 'NONE', #4663, #13556, #8050 ) ;
#5495 = CARTESIAN_POINT ( 'NONE',  ( 2.500000000000000000, 2.357898499370431722, -2.818925648462311528E-15 ) ) ;
#5496 = DIRECTION ( 'NONE',  ( 2.312964634635743450E-16, 1.000000000000000000, 0.000000000000000000 ) ) ;
#5497 = CARTESIAN_POINT ( 'NONE',  ( 219.9999999999999716, -10.00000000000000000, 222.5000000000000853 ) ) ;
#5498 = AXIS2_PLACEMENT_3D ( 'NONE', #5891, #4596, #3646 ) ;
#5499 = AXIS2_PLACEMENT_3D ( 'NONE', #10820, #7537, #5377 ) ;
#5500 = ORIENTED_EDGE ( 'NONE', *, *, #11764, .F. ) ;
#5501 = AXIS2_PLACEMENT_3D ( 'NONE', #2404, #12342, #2547 ) ;
#5502 = DIRECTION ( 'NONE',  ( -0.000000000000000000, 1.000000000000000000, -0.000000000000000000 ) ) ;
#5503 = AXIS2_PLACEMENT_3D ( 'NONE', #11169, #11105, #1135 ) ;
#5504 = VERTEX_POINT ( 'NONE', #9895 ) ;
#5505 = PLANE ( 'NONE',  #3494 ) ;
#5506 = CARTESIAN_POINT ( 'NONE',  ( 5.000000000000004441, 5.204748896376250699E-16, -4.250000000000000000 ) ) ;
#5507 = VERTEX_POINT ( 'NONE', #745 ) ;
#5508 = VERTEX_POINT ( 'NONE', #4458 ) ;
#5510 = EDGE_CURVE ( 'NONE', #8392, #1770, #8879, .T. ) ;
#5509 = CARTESIAN_POINT ( 'NONE',  ( -219.9999999999999147, -85.00000000000009948, 30.00000000000000000 ) ) ;
#5511 = UNCERTAINTY_MEASURE_WITH_UNIT (LENGTH_MEASURE( 1.000000000000000082E-05 ), #6883, 'distance_accuracy_value', 'NONE');
#5512 = EDGE_CURVE ( 'NONE', #5681, #13411, #1325, .T. ) ;
#5513 = VECTOR ( 'NONE', #6080, 1000.000000000000000 ) ;
#5514 = CARTESIAN_POINT ( 'NONE',  ( -4.175002511812151873, -2.208363329454905877, -3.469254087858246738 ) ) ;
#5515 = LINE ( 'NONE', #5846, #9202 ) ;
#5516 = CARTESIAN_POINT ( 'NONE',  ( 170.9999999999999716, 8.660254037844390851, 199.9990000000000236 ) ) ;
#5517 = DIRECTION ( 'NONE',  ( 0.9396926207859138680, 1.150791560227856926E-16, -0.3420201433256536139 ) ) ;
#5518 = DIRECTION ( 'NONE',  ( -0.000000000000000000, 1.000000000000000000, -0.000000000000000000 ) ) ;
#5519 =( LENGTH_UNIT ( ) NAMED_UNIT ( * ) SI_UNIT ( .MILLI., .METRE. ) );
#5520 = DIRECTION ( 'NONE',  ( -1.000000000000000000, 0.000000000000000000, 0.000000000000000000 ) ) ;
#5521 = ITEM_DEFINED_TRANSFORMATION ( 'NONE', 'NONE', #6999,  #14039 ) ;
#5522 = DIRECTION ( 'NONE',  ( 0.000000000000000000, 0.000000000000000000, 1.000000000000000000 ) ) ;
#5523 = ORIENTED_EDGE ( 'NONE', *, *, #8204, .T. ) ;
#5524 = ORIENTED_EDGE ( 'NONE', *, *, #11448, .F. ) ;
#5525 = EDGE_CURVE ( 'NONE', #898, #8647, #2728, .T. ) ;
#5526 = ADVANCED_FACE ( 'NONE', ( #10244 ), #4740, .F. ) ;
#5527 = CARTESIAN_POINT ( 'NONE',  ( 197.5000000000000000, -80.00000000000007105, 55.00000000000001421 ) ) ;
#5528 = ORIENTED_EDGE ( 'NONE', *, *, #5366, .F. ) ;
#5529 = EDGE_CURVE ( 'NONE', #7333, #14219, #6769, .T. ) ;
#5530 = FACE_OUTER_BOUND ( 'NONE', #3989, .T. ) ;
#5531 = CONICAL_SURFACE ( 'NONE', #7634, 2.500000000000002220, 1.029744260000002631 ) ;
#5532 = ORIENTED_EDGE ( 'NONE', *, *, #6667, .F. ) ;
#5533 = CARTESIAN_POINT ( 'NONE',  ( -10.00000000000000000, 0.000000000000000000, 200.0000000000000000 ) ) ;
#5534 = ORIENTED_EDGE ( 'NONE', *, *, #1695, .F. ) ;
#5535 = DIRECTION ( 'NONE',  ( -0.000000000000000000, -0.000000000000000000, 1.000000000000000000 ) ) ;
#5536 = PRODUCT_DEFINITION_SHAPE ( 'NONE', 'NONE',  #14308 ) ;
#5537 = CARTESIAN_POINT ( 'NONE',  ( 219.9999999999999147, -85.00000000000009948, 0.000000000000000000 ) ) ;
#5538 = LINE ( 'NONE', #14159, #836 ) ;
#5539 = CARTESIAN_POINT ( 'NONE',  ( -1.800000000000001155, 1.628780242865979758E-15, 13.29999999999999893 ) ) ;
#5540 = CARTESIAN_POINT ( 'NONE',  ( -1.800000000000002931, 0.000000000000000000, 0.000000000000000000 ) ) ;
#5541 = LINE ( 'NONE', #1017, #6660 ) ;
#5542 = ORIENTED_EDGE ( 'NONE', *, *, #4639, .F. ) ;
#5543 = VECTOR ( 'NONE', #8617, 1000.000000000000000 ) ;
#5544 = ORIENTED_EDGE ( 'NONE', *, *, #13322, .T. ) ;
#5545 = CARTESIAN_POINT ( 'NONE',  ( 132.3499999999999659, -36.99999999999997868, 10.00000000000000000 ) ) ;
#5546 = ORIENTED_EDGE ( 'NONE', *, *, #263, .F. ) ;
#5547 = DIRECTION ( 'NONE',  ( -1.000000000000000000, -0.000000000000000000, -0.000000000000000000 ) ) ;
#5548 = CARTESIAN_POINT ( 'NONE',  ( 297.3499999999999659, -95.00000000000008527, -186.2999999999999829 ) ) ;
#5549 = CARTESIAN_POINT ( 'NONE',  ( 170.9999999999999716, -8.660254037844389075, 200.0000000000000000 ) ) ;
#5550 = ORIENTED_EDGE ( 'NONE', *, *, #4868, .F. ) ;
#5551 = AXIS2_PLACEMENT_3D ( 'NONE', #29, #6518, #2227 ) ;
#5552 = CYLINDRICAL_SURFACE ( 'NONE', #710, 2.500000000000000888 ) ;
#5553 = EDGE_CURVE ( 'NONE', #7253, #13517, #5731, .T. ) ;
#5554 = DIRECTION ( 'NONE',  ( -0.000000000000000000, 0.000000000000000000, 1.000000000000000000 ) ) ;
#5555 = CARTESIAN_POINT ( 'NONE',  ( 82.99999999999998579, -8.660254037844389075, 199.9990000000000236 ) ) ;
#5556 = LINE ( 'NONE', #1032, #12051 ) ;
#5557 = ORIENTED_EDGE ( 'NONE', *, *, #12073, .F. ) ;
#5558 = AXIS2_PLACEMENT_3D ( 'NONE', #10328, #10189, #3665 ) ;
#5559 = CARTESIAN_POINT ( 'NONE',  ( 82.99999999999998579, -8.660254037844389075, 205.0000000000000284 ) ) ;
#5560 = AXIS2_PLACEMENT_3D ( 'NONE', #14254, #2078, #3182 ) ;
#5561 = CARTESIAN_POINT ( 'NONE',  ( -30.00000000000002842, -25.00000000000000000, -169.9999999999999716 ) ) ;
#5562 = AXIS2_PLACEMENT_3D ( 'NONE', #479, #4943, #6094 ) ;
#5563 = CARTESIAN_POINT ( 'NONE',  ( -294.9999999999999432, -75.00000000000008527, 30.00000000000002842 ) ) ;
#5564 = ORIENTED_EDGE ( 'NONE', *, *, #12357, .T. ) ;
#5565 = CARTESIAN_POINT ( 'NONE',  ( 2.000000000000008882, 3.464101615137749945, 0.000000000000000000 ) ) ;
#5566 = FACE_OUTER_BOUND ( 'NONE', #12830, .T. ) ;
#5567 = DIRECTION ( 'NONE',  ( -1.000000000000000000, 0.000000000000000000, 0.000000000000000000 ) ) ;
#5568 = CARTESIAN_POINT ( 'NONE',  ( 386.6666666666666288, -30.00000000000000355, 222.5000000000000853 ) ) ;
#5569 = AXIS2_PLACEMENT_3D ( 'NONE', #11342, #1385, #5896 ) ;
#5570 = CONTEXT_DEPENDENT_SHAPE_REPRESENTATION ( #3273, #13755 ) ;
#5571 = AXIS2_PLACEMENT_3D ( 'NONE', #6812, #2607, #5793 ) ;
#5572 = VERTEX_POINT ( 'NONE', #9229 ) ;
#5573 = EDGE_CURVE ( 'NONE', #5764, #7893, #13370, .T. ) ;
#5574 = CARTESIAN_POINT ( 'NONE',  ( 470.0000000000000000, -20.00000000000000000, 250.0000000000000000 ) ) ;
#5575 = ORIENTED_EDGE ( 'NONE', *, *, #12944, .T. ) ;
#5576 = CARTESIAN_POINT ( 'NONE',  ( 470.0000000000000000, 0.000000000000000000, 205.0000000000000284 ) ) ;
#5577 = EDGE_CURVE ( 'NONE', #9015, #11802, #9450, .T. ) ;
#5578 = VECTOR ( 'NONE', #9252, 1000.000000000000000 ) ;
#5579 = VERTEX_POINT ( 'NONE', #10100 ) ;
#5580 = EDGE_LOOP ( 'NONE', ( #7604, #13788, #11944, #8459 ) ) ;
#5581 = DIRECTION ( 'NONE',  ( 0.000000000000000000, -1.000000000000000000, 1.287488025362403787E-15 ) ) ;
#5582 = DIRECTION ( 'NONE',  ( 1.000000000000000000, 0.000000000000000000, 0.000000000000000000 ) ) ;
#5583 = PLANE ( 'NONE',  #620 ) ;
#5584 = AXIS2_PLACEMENT_3D ( 'NONE', #11491, #2719, #6052 ) ;
#5585 = PLANE ( 'NONE',  #12717 ) ;
#5586 = DIRECTION ( 'NONE',  ( 1.000000000000000000, 0.000000000000000000, 0.000000000000000000 ) ) ;
#5587 = DIRECTION ( 'NONE',  ( -1.000000000000000000, -0.000000000000000000, -0.000000000000000000 ) ) ;
#5588 = DIRECTION ( 'NONE',  ( 0.000000000000000000, 0.000000000000000000, 1.000000000000000000 ) ) ;
#5589 = CARTESIAN_POINT ( 'NONE',  ( 0.000000000000000000, 0.000000000000000000, 200.0000000000000000 ) ) ;
#5590 = VECTOR ( 'NONE', #1853, 1000.000000000000000 ) ;
#5591 = ORIENTED_EDGE ( 'NONE', *, *, #7420, .F. ) ;
#5592 = ORIENTED_EDGE ( 'NONE', *, *, #11142, .F. ) ;
#5593 = EDGE_CURVE ( 'NONE', #11304, #11403, #12489, .T. ) ;
#5594 = CARTESIAN_POINT ( 'NONE',  ( 219.9999999999999716, -15.00000000000000000, 222.5000000000000853 ) ) ;
#5595 = PRODUCT_DEFINITION ( 'UNKNOWN', '', #8389, #11885 ) ;
#5596 = PRESENTATION_LAYER_ASSIGNMENT (  '', '', ( #7480 ) ) ;
#5597 = EDGE_LOOP ( 'NONE', ( #14126, #783, #10410, #2938 ) ) ;
#5598 = VECTOR ( 'NONE', #11199, 1000.000000000000000 ) ;
#5599 = CARTESIAN_POINT ( 'NONE',  ( 224.9999999999999716, -85.00000000000007105, 64.14213562373096522 ) ) ;
#5600 = ORIENTED_EDGE ( 'NONE', *, *, #10191, .T. ) ;
#5601 = DIRECTION ( 'NONE',  ( -0.000000000000000000, -0.000000000000000000, -1.000000000000000000 ) ) ;
#5602 = ORIENTED_EDGE ( 'NONE', *, *, #614, .F. ) ;
#5603 = CARTESIAN_POINT ( 'NONE',  ( 79.99999999999971578, 55.00000000000000711, 10.00000000000000000 ) ) ;
#5604 = CARTESIAN_POINT ( 'NONE',  ( 2.500000000000000000, -2.629050547790028551E-15, -2.041999999999999815 ) ) ;
#5605 = VECTOR ( 'NONE', #7242, 1000.000000000000000 ) ;
#5606 = DIRECTION ( 'NONE',  ( -1.000000000000000000, -0.000000000000000000, -0.000000000000000000 ) ) ;
#5607 = EDGE_CURVE ( 'NONE', #12252, #3295, #277, .T. ) ;
#5608 = EDGE_CURVE ( 'NONE', #6378, #9211, #4669, .T. ) ;
#5609 = DIRECTION ( 'NONE',  ( 1.000000000000000000, 0.000000000000000000, 0.000000000000000000 ) ) ;
#5610 = AXIS2_PLACEMENT_3D ( 'NONE', #12313, #13388, #11158 ) ;
#5611 =( LENGTH_UNIT ( ) NAMED_UNIT ( * ) SI_UNIT ( .MILLI., .METRE. ) );
#5612 = DIRECTION ( 'NONE',  ( 1.000000000000000000, 0.000000000000000000, 0.000000000000000000 ) ) ;
#5613 = CARTESIAN_POINT ( 'NONE',  ( 386.6666666666666288, -25.00000000000000000, -222.5000000000000853 ) ) ;
#5614 = CARTESIAN_POINT ( 'NONE',  ( 201.0000000000000000, -85.00000000000007105, 180.0000000000000000 ) ) ;
#5615 = VERTEX_POINT ( 'NONE', #10309 ) ;
#5616 = EDGE_CURVE ( 'NONE', #11776, #6471, #7913, .T. ) ;
#5617 = ORIENTED_EDGE ( 'NONE', *, *, #64, .F. ) ;
#5618 = AXIS2_PLACEMENT_3D ( 'NONE', #4694, #3532, #12445 ) ;
#5619 = DIRECTION ( 'NONE',  ( 0.000000000000000000, 0.000000000000000000, -1.000000000000000000 ) ) ;
#5620 = AXIS2_PLACEMENT_3D ( 'NONE', #5919, #12455, #10345 ) ;
#5621 = ORIENTED_EDGE ( 'NONE', *, *, #2163, .T. ) ;
#5622 = FACE_OUTER_BOUND ( 'NONE', #813, .T. ) ;
#5623 = CIRCLE ( 'NONE', #8627, 2.649999999999985700 ) ;
#5624 = DIRECTION ( 'NONE',  ( 0.000000000000000000, 0.000000000000000000, 1.000000000000000000 ) ) ;
#5625 = DIRECTION ( 'NONE',  ( -0.8949343913984706411, 0.4461977533473793223, 0.000000000000000000 ) ) ;
#5626 = EDGE_CURVE ( 'NONE', #13531, #3034, #3444, .T. ) ;
#5627 = CARTESIAN_POINT ( 'NONE',  ( 219.9999999999999716, -20.00000000000000000, -225.1500000000000625 ) ) ;
#5628 = EDGE_CURVE ( 'NONE', #8368, #1514, #11302, .T. ) ;
#5629 = DIRECTION ( 'NONE',  ( 0.000000000000000000, -0.4999999999999993894, 0.8660254037844389297 ) ) ;
#5630 = AXIS2_PLACEMENT_3D ( 'NONE', #676, #3896, #1706 ) ;
#5631 = DIRECTION ( 'NONE',  ( 1.000000000000000000, 0.000000000000000000, 0.000000000000000000 ) ) ;
#5632 = CARTESIAN_POINT ( 'NONE',  ( 211.3397459621556038, -90.00000000000007105, 55.00000000000002132 ) ) ;
#5633 = ADVANCED_FACE ( 'NONE', ( #13428, #1456, #342, #8128, #4811, #10173, #12565, #12354, #7845, #12417, #2632, #7049, #11476 ), #10041, .T. ) ;
#5634 = ORIENTED_EDGE ( 'NONE', *, *, #1080, .F. ) ;
#5635 = APPLICATION_CONTEXT ( 'automotive_design' ) ;
#5636 = LINE ( 'NONE', #7935, #2810 ) ;
#5637 = DIRECTION ( 'NONE',  ( 0.000000000000000000, 0.000000000000000000, -1.000000000000000000 ) ) ;
#5638 = CARTESIAN_POINT ( 'NONE',  ( 304.9999999999999432, 45.00000000000001421, 10.00000000000000000 ) ) ;
#5639 = ORIENTED_EDGE ( 'NONE', *, *, #9, .F. ) ;
#5640 = DIRECTION ( 'NONE',  ( 0.000000000000000000, 0.000000000000000000, -1.000000000000000000 ) ) ;
#5641 = CARTESIAN_POINT ( 'NONE',  ( 144.9999999999999716, -64.99999999999997158, 10.00000000000000000 ) ) ;
#5642 = CARTESIAN_POINT ( 'NONE',  ( 303.3333333333333144, -10.00000000000000000, 222.5000000000000853 ) ) ;
#5643 = VERTEX_POINT ( 'NONE', #8944 ) ;
#5644 = CARTESIAN_POINT ( 'NONE',  ( 2.500000000000000000, -2.357898499370432610, 3.252606517456513302E-15 ) ) ;
#5645 = ORIENTED_EDGE ( 'NONE', *, *, #7023, .T. ) ;
#5646 = EDGE_CURVE ( 'NONE', #3491, #3581, #13595, .T. ) ;
#5647 = DIRECTION ( 'NONE',  ( 0.000000000000000000, 1.000000000000000000, -1.471414886128461471E-15 ) ) ;
#5648 = EDGE_LOOP ( 'NONE', ( #8369, #11246, #6545, #654 ) ) ;
#5649 = ORIENTED_EDGE ( 'NONE', *, *, #3449, .F. ) ;
#5650 = CARTESIAN_POINT ( 'NONE',  ( 236.4999999999999432, -85.00000000000007105, 178.4978484569338946 ) ) ;
#5651 = DIRECTION ( 'NONE',  ( -0.000000000000000000, -0.000000000000000000, 1.000000000000000000 ) ) ;
#5652 = CARTESIAN_POINT ( 'NONE',  ( 2.500000000000000000, 0.000000000000000000, 0.000000000000000000 ) ) ;
#5653 = FACE_BOUND ( 'NONE', #1931, .T. ) ;
#5654 = DIRECTION ( 'NONE',  ( -0.000000000000000000, -0.000000000000000000, -1.000000000000000000 ) ) ;
#5655 = CARTESIAN_POINT ( 'NONE',  ( 299.9999999999999432, -75.00000000000008527, -169.9999999999999716 ) ) ;
#5656 = FILL_AREA_STYLE ('',( #2322 ) ) ;
#5657 = LINE ( 'NONE', #111, #9246 ) ;
#5658 = ORIENTED_EDGE ( 'NONE', *, *, #8346, .T. ) ;
#5659 = EDGE_LOOP ( 'NONE', ( #10005, #4557, #8374, #5490, #10155 ) ) ;
#5660 = DIRECTION ( 'NONE',  ( 0.000000000000000000, -1.000000000000000000, -3.491481338843133355E-15 ) ) ;
#5661 = ORIENTED_EDGE ( 'NONE', *, *, #2818, .T. ) ;
#5662 = LINE ( 'NONE', #12478, #4467 ) ;
#5663 = CLOSED_SHELL ( 'NONE', ( #7647, #13693, #11161, #10643, #13584, #9247, #4046, #7128, #7882, #6141, #6242, #12978, #8492, #1980, #5339, #6413, #8533, #10409, #4012, #11415 ) ) ;
#5664 = ORIENTED_EDGE ( 'NONE', *, *, #2566, .F. ) ;
#5665 = CARTESIAN_POINT ( 'NONE',  ( 269.0000000000000000, 8.660254037844390851, 200.0000000000000000 ) ) ;
#5666 = ORIENTED_EDGE ( 'NONE', *, *, #7593, .T. ) ;
#5667 = DIRECTION ( 'NONE',  ( 1.000000000000000000, 0.000000000000000000, 0.000000000000000000 ) ) ;
#5668 = DIRECTION ( 'NONE',  ( -0.000000000000000000, 1.000000000000000000, -0.000000000000000000 ) ) ;
#5669 = CARTESIAN_POINT ( 'NONE',  ( 203.5000000000000000, -85.00000000000007105, 50.00000000000001421 ) ) ;
#5670 = ADVANCED_FACE ( 'NONE', ( #6834 ), #7977, .F. ) ;
#5671 = CARTESIAN_POINT ( 'NONE',  ( 2.000000000000005329, -3.464101615137751722, 0.000000000000000000 ) ) ;
#5672 =( NAMED_UNIT ( * ) PLANE_ANGLE_UNIT ( ) SI_UNIT ( $, .RADIAN. ) );
#5673 = ADVANCED_FACE ( 'NONE', ( #6034 ), #11620, .F. ) ;
#5674 = DIRECTION ( 'NONE',  ( -0.000000000000000000, -0.000000000000000000, 1.000000000000000000 ) ) ;
#5675 = CARTESIAN_POINT ( 'NONE',  ( 2.740000000000000213, -0.9838866223905674557, -0.5150000000000000133 ) ) ;
#5676 = ORIENTED_EDGE ( 'NONE', *, *, #7087, .T. ) ;
#5677 = AXIS2_PLACEMENT_3D ( 'NONE', #8145, #13516, #2648 ) ;
#5678 = ORIENTED_EDGE ( 'NONE', *, *, #4535, .F. ) ;
#5679 = VERTEX_POINT ( 'NONE', #5027 ) ;
#5680 = CARTESIAN_POINT ( 'NONE',  ( 170.9999999999999716, 8.660254037844390851, 200.0000000000000000 ) ) ;
#5681 = VERTEX_POINT ( 'NONE', #1594 ) ;
#5682 = DIRECTION ( 'NONE',  ( 0.8949343913984143528, 0.4461977533474921764, 1.416481476476136321E-16 ) ) ;
#5683 = DIRECTION ( 'NONE',  ( 0.000000000000000000, 0.5000000000000011102, 0.8660254037844379305 ) ) ;
#5684 = AXIS2_PLACEMENT_3D ( 'NONE', #3198, #10881, #2092 ) ;
#5685 = EDGE_CURVE ( 'NONE', #806, #611, #8348, .T. ) ;
#5686 = CARTESIAN_POINT ( 'NONE',  ( 259.0000000000000000, -8.660254037844389075, 200.0000000000000000 ) ) ;
#5687 = CARTESIAN_POINT ( 'NONE',  ( 0.000000000000000000, 2.357898499370433054, -1.951563910473907981E-15 ) ) ;
#5688 = DIRECTION ( 'NONE',  ( 1.000000000000000000, 0.000000000000000000, 0.000000000000000000 ) ) ;
#5689 = CARTESIAN_POINT ( 'NONE',  ( 0.000000000000000000, 0.000000000000000000, 10.00000000000000000 ) ) ;
#5690 = ADVANCED_FACE ( 'NONE', ( #564 ), #10385, .F. ) ;
#5691 = EDGE_LOOP ( 'NONE', ( #7337, #955 ) ) ;
#5692 = VECTOR ( 'NONE', #11469, 1000.000000000000000 ) ;
#5693 = EDGE_CURVE ( 'NONE', #5507, #4511, #7348, .T. ) ;
#5694 = EDGE_CURVE ( 'NONE', #10615, #1243, #9375, .T. ) ;
#5695 = ADVANCED_FACE ( 'NONE', ( #11690 ), #13137, .T. ) ;
#5696 = DIRECTION ( 'NONE',  ( 0.000000000000000000, 0.000000000000000000, 1.000000000000000000 ) ) ;
#5697 = LINE ( 'NONE', #13381, #7231 ) ;
#5698 = LINE ( 'NONE', #1192, #7354 ) ;
#5699 = ORIENTED_EDGE ( 'NONE', *, *, #5774, .F. ) ;
#5700 = VECTOR ( 'NONE', #9272, 1000.000000000000000 ) ;
#5701 = CARTESIAN_POINT ( 'NONE',  ( 219.9999999999999716, -85.00000000000007105, 170.0000000000000000 ) ) ;
#5702 = VECTOR ( 'NONE', #6273, 1000.000000000000000 ) ;
#5703 = FACE_BOUND ( 'NONE', #2386, .T. ) ;
#5704 = DIRECTION ( 'NONE',  ( 1.000000000000000000, 6.123233995736766036E-17, -6.123233995736764803E-17 ) ) ;
#5705 = AXIS2_PLACEMENT_3D ( 'NONE', #12057, #7483, #10757 ) ;
#5706 = VERTEX_POINT ( 'NONE', #4073 ) ;
#5707 = AXIS2_PLACEMENT_3D ( 'NONE', #7074, #13602, #13812 ) ;
#5708 = DIRECTION ( 'NONE',  ( 1.000000000000000000, 0.000000000000000000, 0.000000000000000000 ) ) ;
#5709 = AXIS2_PLACEMENT_3D ( 'NONE', #8068, #13254, #13318 ) ;
#5710 = VERTEX_POINT ( 'NONE', #11768 ) ;
#5711 = PLANE ( 'NONE',  #8585 ) ;
#5712 = CIRCLE ( 'NONE', #5501, 2.649999999999985700 ) ;
#5713 = ORIENTED_EDGE ( 'NONE', *, *, #4069, .F. ) ;
#5714 = ORIENTED_EDGE ( 'NONE', *, *, #3116, .T. ) ;
#5715 = DIRECTION ( 'NONE',  ( 0.000000000000000000, 0.000000000000000000, -1.000000000000000000 ) ) ;
#5716 = CARTESIAN_POINT ( 'NONE',  ( -2.756197834950067094, -3.027510591568735254, -3.223146290109809797 ) ) ;
#5717 = VECTOR ( 'NONE', #11420, 1000.000000000000000 ) ;
#5718 = FACE_OUTER_BOUND ( 'NONE', #4679, .T. ) ;
#5719 = LINE ( 'NONE', #2455, #6730 ) ;
#5720 = VECTOR ( 'NONE', #61, 1000.000000000000000 ) ;
#5721 = CARTESIAN_POINT ( 'NONE',  ( 119.9999999999999147, -225.0010000000000048, -169.9999999999999716 ) ) ;
#5722 = CARTESIAN_POINT ( 'NONE',  ( 197.5000000000000000, -90.00000000000007105, 55.00000000000001421 ) ) ;
#5723 = ADVANCED_FACE ( 'NONE', ( #415 ), #5288, .F. ) ;
#5724 = FACE_OUTER_BOUND ( 'NONE', #8421, .T. ) ;
#5725 = ITEM_DEFINED_TRANSFORMATION ( 'NONE', 'NONE', #4463,  #14039 ) ;
#5726 = AXIS2_PLACEMENT_3D ( 'NONE', #3501, #197, #5950 ) ;
#5727 = AXIS2_PLACEMENT_3D ( 'NONE', #4802, #8121, #5813 ) ;
#5728 = ORIENTED_EDGE ( 'NONE', *, *, #4117, .F. ) ;
#5729 = ORIENTED_EDGE ( 'NONE', *, *, #7357, .T. ) ;
#5730 = DIRECTION ( 'NONE',  ( -1.000000000000000000, 0.000000000000000000, 0.000000000000000000 ) ) ;
#5731 = CIRCLE ( 'NONE', #5498, 9.999999999999994671 ) ;
#5732 = ORIENTED_EDGE ( 'NONE', *, *, #9957, .T. ) ;
#5733 = DIRECTION ( 'NONE',  ( 0.000000000000000000, 1.000000000000000000, 0.000000000000000000 ) ) ;
#5734 = CONICAL_SURFACE ( 'NONE', #6895, 2.500000000000002220, 1.029744260000002631 ) ;
#5735 = ORIENTED_EDGE ( 'NONE', *, *, #1501, .T. ) ;
#5736 = DIRECTION ( 'NONE',  ( 0.000000000000000000, 0.000000000000000000, -1.000000000000000000 ) ) ;
#5737 = VERTEX_POINT ( 'NONE', #5964 ) ;
#5738 = DIRECTION ( 'NONE',  ( 1.000000000000000000, 0.000000000000000000, 0.000000000000000000 ) ) ;
#5739 = AXIS2_PLACEMENT_3D ( 'NONE', #8525, #14172, #13167 ) ;
#5740 = CARTESIAN_POINT ( 'NONE',  ( -294.9999999999999432, 55.00000000000001421, 40.00000000000000000 ) ) ;
#5741 = SURFACE_STYLE_USAGE ( .BOTH. , #11195 ) ;
#5742 = DIRECTION ( 'NONE',  ( -0.000000000000000000, -0.000000000000000000, -1.000000000000000000 ) ) ;
#5743 =( NAMED_UNIT ( * ) PLANE_ANGLE_UNIT ( ) SI_UNIT ( $, .RADIAN. ) );
#5744 = DIRECTION ( 'NONE',  ( -0.000000000000000000, 1.000000000000000000, -0.000000000000000000 ) ) ;
#5745 = CARTESIAN_POINT ( 'NONE',  ( 304.9999999999999432, 45.00000000000001421, -174.9999999999999716 ) ) ;
#5746 = DIRECTION ( 'NONE',  ( -1.000000000000000000, -0.000000000000000000, -0.000000000000000000 ) ) ;
#5747 = EDGE_LOOP ( 'NONE', ( #7622, #4444, #13530, #9438 ) ) ;
#5748 = MECHANICAL_DESIGN_GEOMETRIC_PRESENTATION_REPRESENTATION (  '', ( #10149 ), #636 ) ;
#5749 = ORIENTED_EDGE ( 'NONE', *, *, #13390, .T. ) ;
#5750 = ORIENTED_EDGE ( 'NONE', *, *, #10671, .F. ) ;
#5751 = EDGE_CURVE ( 'NONE', #8946, #7668, #148, .T. ) ;
#5752 = DIRECTION ( 'NONE',  ( -1.000000000000000000, 0.000000000000000000, 0.000000000000000000 ) ) ;
#5753 = ORIENTED_EDGE ( 'NONE', *, *, #3456, .F. ) ;
#5754 = FACE_BOUND ( 'NONE', #155, .T. ) ;
#5755 = LINE ( 'NONE', #12364, #1538 ) ;
#5756 = CARTESIAN_POINT ( 'NONE',  ( 134.9999999999999432, -56.99999999999997158, 10.00000000000000000 ) ) ;
#5757 =( REPRESENTATION_RELATIONSHIP ('NONE','NONE', #11251, #2275 ) REPRESENTATION_RELATIONSHIP_WITH_TRANSFORMATION ( #10878 )SHAPE_REPRESENTATION_RELATIONSHIP( ) );
#5758 = DIRECTION ( 'NONE',  ( -0.000000000000000000, -0.000000000000000000, -1.000000000000000000 ) ) ;
#5759 = DIRECTION ( 'NONE',  ( -1.000000000000000000, -0.000000000000000000, -0.000000000000000000 ) ) ;
#5760 = CIRCLE ( 'NONE', #3003, 2.649999999999985700 ) ;
#5761 = DIRECTION ( 'NONE',  ( 0.000000000000000000, 0.000000000000000000, 1.000000000000000000 ) ) ;
#5762 = PRODUCT_DEFINITION_SHAPE ( 'NONE', 'NONE',  #14321 ) ;
#5763 = LINE ( 'NONE', #7860, #8691 ) ;
#5764 = VERTEX_POINT ( 'NONE', #13998 ) ;
#5765 = EDGE_CURVE ( 'NONE', #1149, #2677, #174, .T. ) ;
#5766 = FILL_AREA_STYLE_COLOUR ( '', #10253 ) ;
#5767 = PRODUCT_DEFINITION ( 'UNKNOWN', '', #1438, #9711 ) ;
#5768 = CARTESIAN_POINT ( 'NONE',  ( -30.00000000000002842, -20.00000000000000000, 250.0000000000000000 ) ) ;
#5769 = AXIS2_PLACEMENT_3D ( 'NONE', #12239, #10063, #1266 ) ;
#5770 = FACE_OUTER_BOUND ( 'NONE', #14152, .T. ) ;
#5771 = DIRECTION ( 'NONE',  ( 0.000000000000000000, -0.000000000000000000, 1.000000000000000000 ) ) ;
#5772 = ORIENTED_EDGE ( 'NONE', *, *, #340, .T. ) ;
#5773 = CARTESIAN_POINT ( 'NONE',  ( -12.00000000000000000, 0.000000000000000000, -186.0000000000000000 ) ) ;
#5774 = EDGE_CURVE ( 'NONE', #7639, #13552, #2023, .T. ) ;
#5775 = ADVANCED_FACE ( 'NONE', ( #1740, #12923 ), #7332, .F. ) ;
#5776 = DIRECTION ( 'NONE',  ( 1.000000000000000000, 0.000000000000000000, 0.000000000000000000 ) ) ;
#5777 = DIRECTION ( 'NONE',  ( 0.000000000000000000, 0.000000000000000000, 1.000000000000000000 ) ) ;
#5778 = EDGE_CURVE ( 'NONE', #3164, #4582, #12909, .T. ) ;
#5779 = VECTOR ( 'NONE', #11144, 1000.000000000000000 ) ;
#5780 =( BOUNDED_SURFACE ( )  B_SPLINE_SURFACE ( 3, 2, ( 
 ( #922, #3216, #6394 ),
 ( #6327, #1962, #4148 ),
 ( #5315, #4440, #6607 ),
 ( #9874, #7542, #9738 ),
 ( #8785, #11914, #13207 ),
 ( #10974, #8710, #14144 ) ),
 .UNSPECIFIED., .F., .F., .F. ) 
 B_SPLINE_SURFACE_WITH_KNOTS ( ( 4, 2, 4 ),
 ( 3, 3 ),
 ( 0.02027752710269158445, 0.02273781595091097299, 0.02519810479913036153 ),
 ( 0.000000000000000000, 1.000000000000000000 ),
 .UNSPECIFIED. ) 
 GEOMETRIC_REPRESENTATION_ITEM ( )  RATIONAL_B_SPLINE_SURFACE ( (
 ( 1.000000000000000000, 0.8047781431712808242, 1.000000000000000000),
 ( 1.000000000000000000, 0.8123773247083928561, 1.000000000000000000),
 ( 1.000000000000000000, 0.8190670192154906326, 1.000000000000000000),
 ( 1.000000000000000000, 0.8192353552912178261, 1.000000000000000000),
 ( 1.000000000000000000, 0.8126132098226825917, 1.000000000000000000),
 ( 1.000000000000000000, 0.8047712465856394770, 1.000000000000000000) ) ) 
 REPRESENTATION_ITEM ( '' )  SURFACE ( )  );
#5781 = VECTOR ( 'NONE', #4559, 1000.000000000000000 ) ;
#5782 = AXIS2_PLACEMENT_3D ( 'NONE', #8230, #12662, #4988 ) ;
#5783 = ORIENTED_EDGE ( 'NONE', *, *, #9393, .T. ) ;
#5784 = DIRECTION ( 'NONE',  ( 0.000000000000000000, 0.000000000000000000, -1.000000000000000000 ) ) ;
#5785 = ORIENTED_EDGE ( 'NONE', *, *, #7456, .T. ) ;
#5786 = DIRECTION ( 'NONE',  ( -0.000000000000000000, -0.000000000000000000, 1.000000000000000000 ) ) ;
#5787 = ORIENTED_EDGE ( 'NONE', *, *, #947, .T. ) ;
#5788 = ORIENTED_EDGE ( 'NONE', *, *, #12301, .F. ) ;
#5789 = CARTESIAN_POINT ( 'NONE',  ( 53.33333333333330017, -25.00000000000000000, -219.8500000000001080 ) ) ;
#5790 = LINE ( 'NONE', #13614, #8001 ) ;
#5791 = AXIS2_PLACEMENT_3D ( 'NONE', #10539, #6043, #7338 ) ;
#5792 = DIRECTION ( 'NONE',  ( -0.000000000000000000, -1.000000000000000000, -0.000000000000000000 ) ) ;
#5793 = DIRECTION ( 'NONE',  ( 0.000000000000000000, 0.000000000000000000, 1.000000000000000000 ) ) ;
#5794 = CARTESIAN_POINT ( 'NONE',  ( 132.4999999999999432, -36.99999999999997868, -180.0000000000000000 ) ) ;
#5795 = DIRECTION ( 'NONE',  ( -1.000000000000000000, -9.912705577010325549E-17, 0.000000000000000000 ) ) ;
#5796 = SHAPE_REPRESENTATION_RELATIONSHIP ( 'NONE' , 'NONE' ,  #3385, #5258 ) ;
#5797 = EDGE_CURVE ( 'NONE', #1004, #8679, #8754, .T. ) ;
#5798 = CIRCLE ( 'NONE', #8821, 2.649999999999985700 ) ;
#5799 = CARTESIAN_POINT ( 'NONE',  ( 132.3499999999999659, -56.99999999999997158, 0.000000000000000000 ) ) ;
#5800 = CONTEXT_DEPENDENT_SHAPE_REPRESENTATION ( #13442, #10407 ) ;
#5801 = EDGE_LOOP ( 'NONE', ( #1226, #3435, #11245, #4713 ) ) ;
#5802 = ORIENTED_EDGE ( 'NONE', *, *, #9569, .T. ) ;
#5803 = EDGE_CURVE ( 'NONE', #9645, #1558, #13152, .T. ) ;
#5804 = LINE ( 'NONE', #10085, #11941 ) ;
#5805 = VECTOR ( 'NONE', #4047, 1000.000000000000000 ) ;
#5806 = ORIENTED_EDGE ( 'NONE', *, *, #894, .F. ) ;
#5807 = CARTESIAN_POINT ( 'NONE',  ( 0.000000000000000000, 0.000000000000000000, -4.694516984716113228 ) ) ;
#5808 = EDGE_LOOP ( 'NONE', ( #10571, #6102, #12268, #3079, #5171 ) ) ;
#5809 = CARTESIAN_POINT ( 'NONE',  ( 53.33333333333330017, -20.00000000000000000, -222.5000000000000853 ) ) ;
#5810 = ORIENTED_EDGE ( 'NONE', *, *, #2658, .T. ) ;
#5811 = MECHANICAL_DESIGN_GEOMETRIC_PRESENTATION_REPRESENTATION (  '', ( #12530 ), #14150 ) ;
#5812 = CARTESIAN_POINT ( 'NONE',  ( 222.4999999999999147, -85.00000000000009948, 0.000000000000000000 ) ) ;
#5813 = DIRECTION ( 'NONE',  ( -1.000000000000000000, 0.000000000000000000, 0.000000000000000000 ) ) ;
#5814 = ORIENTED_EDGE ( 'NONE', *, *, #2447, .F. ) ;
#5815 = CARTESIAN_POINT ( 'NONE',  ( 25.00000000000000000, 2.789133085058098087E-16, -2.055000000000000160 ) ) ;
#5816 = FACE_OUTER_BOUND ( 'NONE', #8983, .T. ) ;
#5817 = CIRCLE ( 'NONE', #7663, 2.500000000000002220 ) ;
#5818 =( LENGTH_UNIT ( ) NAMED_UNIT ( * ) SI_UNIT ( .MILLI., .METRE. ) );
#5819 = DIRECTION ( 'NONE',  ( 1.000000000000000000, 0.000000000000000000, 0.000000000000000000 ) ) ;
#5820 =( REPRESENTATION_RELATIONSHIP ('NONE','NONE', #11251, #208 ) REPRESENTATION_RELATIONSHIP_WITH_TRANSFORMATION ( #14076 )SHAPE_REPRESENTATION_RELATIONSHIP( ) );
#5821 = EDGE_LOOP ( 'NONE', ( #6114, #3410, #8132, #14019, #8765, #9726, #6184, #12654, #4076, #7270, #9982, #1944 ) ) ;
#5822 = EDGE_LOOP ( 'NONE', ( #2796, #6073, #304 ) ) ;
#5823 = VERTEX_POINT ( 'NONE', #2916 ) ;
#5824 = DIRECTION ( 'NONE',  ( 0.000000000000000000, 0.000000000000000000, 1.000000000000000000 ) ) ;
#5825 = AXIS2_PLACEMENT_3D ( 'NONE', #14175, #814, #11797 ) ;
#5826 = EDGE_CURVE ( 'NONE', #6215, #5006, #6250, .T. ) ;
#5827 = EDGE_LOOP ( 'NONE', ( #9158, #9805, #933, #2903 ) ) ;
#5828 = DIRECTION ( 'NONE',  ( -0.000000000000000000, 0.000000000000000000, -1.000000000000000000 ) ) ;
#5829 = ORIENTED_EDGE ( 'NONE', *, *, #2230, .T. ) ;
#5830 = FACE_BOUND ( 'NONE', #7021, .T. ) ;
#5831 =( GEOMETRIC_REPRESENTATION_CONTEXT ( 3 ) GLOBAL_UNCERTAINTY_ASSIGNED_CONTEXT ( ( #7678 ) ) GLOBAL_UNIT_ASSIGNED_CONTEXT ( ( #10513, #11386, #6954 ) ) REPRESENTATION_CONTEXT ( 'NONE', 'WORKASPACE' ) );
#5832 = DIRECTION ( 'NONE',  ( -0.000000000000000000, -0.000000000000000000, 1.000000000000000000 ) ) ;
#5833 = DIRECTION ( 'NONE',  ( 0.000000000000000000, 0.000000000000000000, -1.000000000000000000 ) ) ;
#5834 = DIRECTION ( 'NONE',  ( -0.000000000000000000, -0.000000000000000000, 1.000000000000000000 ) ) ;
#5835 = DIRECTION ( 'NONE',  ( -0.000000000000000000, -0.000000000000000000, 1.000000000000000000 ) ) ;
#5836 = CARTESIAN_POINT ( 'NONE',  ( 0.000000000000000000, -1.178949249685214307, 2.042000000000001592 ) ) ;
#5837 = AXIS2_PLACEMENT_3D ( 'NONE', #13583, #3875, #3662 ) ;
#5838 = CARTESIAN_POINT ( 'NONE',  ( 136.6666666666666288, -20.00000000000000000, 222.5000000000000853 ) ) ;
#5839 = VERTEX_POINT ( 'NONE', #9665 ) ;
#5840 = AXIS2_PLACEMENT_3D ( 'NONE', #12817, #11658, #3108 ) ;
#5841 = VECTOR ( 'NONE', #3630, 1000.000000000000000 ) ;
#5842 = LINE ( 'NONE', #11571, #7878 ) ;
#5843 = LINE ( 'NONE', #7936, #13260 ) ;
#5844 = FACE_OUTER_BOUND ( 'NONE', #2235, .T. ) ;
#5845 = ORIENTED_EDGE ( 'NONE', *, *, #7366, .T. ) ;
#5846 = CARTESIAN_POINT ( 'NONE',  ( 79.99999999999971578, 35.00000000000000000, 10.00000000000000000 ) ) ;
#5847 = DIRECTION ( 'NONE',  ( 0.000000000000000000, 0.000000000000000000, 1.000000000000000000 ) ) ;
#5848 = EDGE_CURVE ( 'NONE', #8299, #3017, #4700, .T. ) ;
#5849 = DIRECTION ( 'NONE',  ( -1.000000000000000000, -0.000000000000000000, -0.000000000000000000 ) ) ;
#5850 = DIRECTION ( 'NONE',  ( 6.123233995736766036E-17, -1.000000000000000000, 0.000000000000000000 ) ) ;
#5851 = EDGE_CURVE ( 'NONE', #11376, #8753, #6204, .T. ) ;
#5852 = DIRECTION ( 'NONE',  ( -1.000000000000000000, 0.000000000000000000, -0.000000000000000000 ) ) ;
#5853 = CIRCLE ( 'NONE', #13964, 2.649999999999985700 ) ;
#5854 = EDGE_LOOP ( 'NONE', ( #13649, #482, #2634, #12848 ) ) ;
#5855 = CARTESIAN_POINT ( 'NONE',  ( 2.000000000000000444, 3.464101615137754830, -3.142992957459231018 ) ) ;
#5856 = AXIS2_PLACEMENT_3D ( 'NONE', #13608, #10350, #3971 ) ;
#5857 = ORIENTED_EDGE ( 'NONE', *, *, #3151, .T. ) ;
#5858 = CARTESIAN_POINT ( 'NONE',  ( 303.3333333333333144, -15.00000000000000000, 219.8500000000001080 ) ) ;
#5859 = ADVANCED_FACE ( 'NONE', ( #11983 ), #12123, .F. ) ;
#5860 = ORIENTED_EDGE ( 'NONE', *, *, #214, .F. ) ;
#5861 = ORIENTED_EDGE ( 'NONE', *, *, #5273, .T. ) ;
#5862 = DIRECTION ( 'NONE',  ( -0.000000000000000000, -0.000000000000000000, 1.000000000000000000 ) ) ;
#5863 = CARTESIAN_POINT ( 'NONE',  ( 2.742827927723449299, 3.035229711104609596, -3.433252694550591233 ) ) ;
#5864 = LINE ( 'NONE', #1715, #7817 ) ;
#5865 = EDGE_CURVE ( 'NONE', #8193, #3237, #5056, .T. ) ;
#5866 = DIRECTION ( 'NONE',  ( 0.000000000000000000, 0.000000000000000000, -1.000000000000000000 ) ) ;
#5867 = CARTESIAN_POINT ( 'NONE',  ( 360.0000000000000000, 55.00000000000001421, 10.00000000000000000 ) ) ;
#5868 = LINE ( 'NONE', #9204, #11061 ) ;
#5869 = FILL_AREA_STYLE ('',( #3768 ) ) ;
#5870 = CARTESIAN_POINT ( 'NONE',  ( 2.500000000000000000, 0.000000000000000000, 0.000000000000000000 ) ) ;
#5871 = VERTEX_POINT ( 'NONE', #1000 ) ;
#5872 = VERTEX_POINT ( 'NONE', #5448 ) ;
#5873 = DIRECTION ( 'NONE',  ( 0.000000000000000000, -3.491481338843133355E-15, 1.000000000000000000 ) ) ;
#5874 = VERTEX_POINT ( 'NONE', #7686 ) ;
#5875 = FACE_OUTER_BOUND ( 'NONE', #1010, .T. ) ;
#5876 = EDGE_CURVE ( 'NONE', #13361, #9311, #11734, .T. ) ;
#5877 = EDGE_CURVE ( 'NONE', #5408, #3025, #2183, .T. ) ;
#5878 = ORIENTED_EDGE ( 'NONE', *, *, #6771, .T. ) ;
#5879 = ADVANCED_FACE ( 'NONE', ( #10897 ), #5780, .F. ) ;
#5880 = LINE ( 'NONE', #13419, #11078 ) ;
#5881 = VERTEX_POINT ( 'NONE', #5241 ) ;
#5882 = EDGE_CURVE ( 'NONE', #5322, #2121, #14265, .T. ) ;
#5883 = CARTESIAN_POINT ( 'NONE',  ( 219.9999999999999716, -20.00000000000000000, 222.5000000000000853 ) ) ;
#5884 = CARTESIAN_POINT ( 'NONE',  ( -5.000000000000000888, -8.660254037844389075, 210.0000000000000000 ) ) ;
#5885 = EDGE_LOOP ( 'NONE', ( #2333, #5142, #10233, #4390 ) ) ;
#5886 = LINE ( 'NONE', #10037, #2952 ) ;
#5887 = EDGE_CURVE ( 'NONE', #3798, #12343, #10252, .T. ) ;
#5888 = CARTESIAN_POINT ( 'NONE',  ( -2.000000000000007550, -3.464101615137749945, 0.000000000000000000 ) ) ;
#5889 = SURFACE_STYLE_USAGE ( .BOTH. , #10242 ) ;
#5890 = SHAPE_DEFINITION_REPRESENTATION ( #291, #9778 ) ;
#5891 = CARTESIAN_POINT ( 'NONE',  ( 1.799999999999996048, 0.000000000000000000, 0.000000000000000000 ) ) ;
#5892 = ORIENTED_EDGE ( 'NONE', *, *, #3914, .F. ) ;
#5893 = ORIENTED_EDGE ( 'NONE', *, *, #4470, .F. ) ;
#5894 = AXIS2_PLACEMENT_3D ( 'NONE', #7526, #5302, #10739 ) ;
#5895 = ORIENTED_EDGE ( 'NONE', *, *, #2122, .T. ) ;
#5896 = DIRECTION ( 'NONE',  ( 1.000000000000000000, 0.000000000000000000, 0.000000000000000000 ) ) ;
#5897 = EDGE_LOOP ( 'NONE', ( #13879, #7656, #3586, #8202 ) ) ;
#5898 = CARTESIAN_POINT ( 'NONE',  ( -31.74999999999995737, 0.000000000000000000, 0.000000000000000000 ) ) ;
#5899 = ORIENTED_EDGE ( 'NONE', *, *, #6398, .T. ) ;
#5900 = DIRECTION ( 'NONE',  ( 0.000000000000000000, 1.000000000000000000, 0.000000000000000000 ) ) ;
#5901 = CARTESIAN_POINT ( 'NONE',  ( 0.06760930072668799862, 0.5149999999999969047, 0.9010842325122926377 ) ) ;
#5902 = DIRECTION ( 'NONE',  ( 1.000000000000000000, 0.000000000000000000, 0.000000000000000000 ) ) ;
#5903 = CLOSED_SHELL ( 'NONE', ( #2427, #13748, #7827, #2398, #886, #4473, #7300, #8174, #9260, #2774, #13287, #6379 ) ) ;
#5904 = LINE ( 'NONE', #10326, #4913 ) ;
#5905 = CYLINDRICAL_SURFACE ( 'NONE', #11609, 5.500000000000005329 ) ;
#5906 = LINE ( 'NONE', #12509, #13655 ) ;
#5907 = DIRECTION ( 'NONE',  ( 0.000000000000000000, 0.000000000000000000, -1.000000000000000000 ) ) ;
#5908 = EDGE_CURVE ( 'NONE', #1839, #3111, #6170, .T. ) ;
#5909 = ORIENTED_EDGE ( 'NONE', *, *, #308, .F. ) ;
#5910 =( NAMED_UNIT ( * ) SI_UNIT ( $, .STERADIAN. ) SOLID_ANGLE_UNIT ( ) );
#5911 = VECTOR ( 'NONE', #2617, 1000.000000000000000 ) ;
#5912 = DIRECTION ( 'NONE',  ( 0.000000000000000000, 0.000000000000000000, 1.000000000000000000 ) ) ;
#5913 = DIRECTION ( 'NONE',  ( -0.000000000000000000, -0.000000000000000000, -1.000000000000000000 ) ) ;
#5914 = LINE ( 'NONE', #12652, #7582 ) ;
#5915 = ORIENTED_EDGE ( 'NONE', *, *, #11473, .F. ) ;
#5916 = DIRECTION ( 'NONE',  ( -1.000000000000000000, -0.000000000000000000, -0.000000000000000000 ) ) ;
#5917 = CIRCLE ( 'NONE', #9402, 5.384454397937118664 ) ;
#5918 = DIRECTION ( 'NONE',  ( -0.000000000000000000, -1.000000000000000000, -0.000000000000000000 ) ) ;
#5919 = CARTESIAN_POINT ( 'NONE',  ( 264.0000000000000000, 0.000000000000000000, 0.000000000000000000 ) ) ;
#5920 = EDGE_CURVE ( 'NONE', #4912, #2540, #9656, .T. ) ;
#5921 = CARTESIAN_POINT ( 'NONE',  ( 0.06760930072668894231, -0.9010842325122929708, -0.5150000000000000133 ) ) ;
#5922 = ORIENTED_EDGE ( 'NONE', *, *, #12648, .F. ) ;
#5923 = CARTESIAN_POINT ( 'NONE',  ( 8.000000000000000000, -4.837354856632045452E-15, 0.000000000000000000 ) ) ;
#5924 = DIRECTION ( 'NONE',  ( 0.000000000000000000, 0.000000000000000000, -1.000000000000000000 ) ) ;
#5925 = EDGE_CURVE ( 'NONE', #13138, #11936, #9176, .T. ) ;
#5926 = AXIS2_PLACEMENT_3D ( 'NONE', #1952, #10964, #10677 ) ;
#5927 = VERTEX_POINT ( 'NONE', #782 ) ;
#5928 = ADVANCED_BREP_SHAPE_REPRESENTATION ( '', ( #8659, #14039 ), #3976 ) ;
#5929 = DIRECTION ( 'NONE',  ( 1.000000000000000000, 0.000000000000000000, 0.000000000000000000 ) ) ;
#5930 =( GEOMETRIC_REPRESENTATION_CONTEXT ( 3 ) GLOBAL_UNCERTAINTY_ASSIGNED_CONTEXT ( ( #796 ) ) GLOBAL_UNIT_ASSIGNED_CONTEXT ( ( #759, #615, #1865 ) ) REPRESENTATION_CONTEXT ( 'NONE', 'WORKASPACE' ) );
#5931 = LINE ( 'NONE', #7883, #1521 ) ;
#5932 = DIRECTION ( 'NONE',  ( -1.000000000000000000, -0.000000000000000000, -0.000000000000000000 ) ) ;
#5933 = DIRECTION ( 'NONE',  ( 1.000000000000000000, 0.000000000000000000, 0.000000000000000000 ) ) ;
#5934 = CARTESIAN_POINT ( 'NONE',  ( 17.00000000000000000, 0.000000000000000000, 2.055000000000000160 ) ) ;
#5935 = DIRECTION ( 'NONE',  ( 0.000000000000000000, 0.000000000000000000, 1.000000000000000000 ) ) ;
#5936 = SURFACE_STYLE_FILL_AREA ( #5869 ) ;
#5937 = VECTOR ( 'NONE', #5518, 1000.000000000000000 ) ;
#5938 = CARTESIAN_POINT ( 'NONE',  ( 2.000000000000008882, 3.464101615137749945, 0.000000000000000000 ) ) ;
#5939 = CIRCLE ( 'NONE', #4093, 5.500000000000005329 ) ;
#5940 = ITEM_DEFINED_TRANSFORMATION ( 'NONE', 'NONE', #6304,  #14039 ) ;
#5941 = EDGE_LOOP ( 'NONE', ( #6267, #11551, #3625, #11612 ) ) ;
#5942 = ORIENTED_EDGE ( 'NONE', *, *, #1782, .T. ) ;
#5943 = FACE_OUTER_BOUND ( 'NONE', #4873, .T. ) ;
#5944 = EDGE_LOOP ( 'NONE', ( #13398, #9961, #9917, #9595 ) ) ;
#5945 = DIRECTION ( 'NONE',  ( -1.000000000000000000, -0.000000000000000000, -0.000000000000000000 ) ) ;
#5946 = EDGE_CURVE ( 'NONE', #4174, #13795, #13108, .T. ) ;
#5947 = PRODUCT_RELATED_PRODUCT_CATEGORY ( 'part', '', ( #7839 ) ) ;
#5948 = AXIS2_PLACEMENT_3D ( 'NONE', #316, #9131, #11317 ) ;
#5949 = ORIENTED_EDGE ( 'NONE', *, *, #2670, .T. ) ;
#5950 = DIRECTION ( 'NONE',  ( -1.000000000000000000, 0.000000000000000000, 0.000000000000000000 ) ) ;
#5951 = EDGE_LOOP ( 'NONE', ( #11327, #3252, #13727 ) ) ;
#5952 = LINE ( 'NONE', #4800, #100 ) ;
#5953 = AXIS2_PLACEMENT_3D ( 'NONE', #8583, #4452, #7559 ) ;
#5954 = CARTESIAN_POINT ( 'NONE',  ( 269.0000000000000000, 8.660254037844390851, 199.9990000000000236 ) ) ;
#5955 = EDGE_LOOP ( 'NONE', ( #2204, #13752 ) ) ;
#5956 = CARTESIAN_POINT ( 'NONE',  ( -1.800000000000001155, 0.000000000000000000, 0.000000000000000000 ) ) ;
#5957 = VECTOR ( 'NONE', #7764, 1000.000000000000000 ) ;
#5958 = DIRECTION ( 'NONE',  ( 0.000000000000000000, 0.000000000000000000, 1.000000000000000000 ) ) ;
#5959 = VECTOR ( 'NONE', #3086, 1000.000000000000114 ) ;
#5960 = PLANE ( 'NONE',  #1403 ) ;
#5961 = PRODUCT_CONTEXT ( 'NONE', #2114, 'mechanical' ) ;
#5962 = EDGE_CURVE ( 'NONE', #1312, #7893, #527, .T. ) ;
#5963 = ADVANCED_FACE ( 'NONE', ( #7828 ), #13751, .F. ) ;
#5964 = CARTESIAN_POINT ( 'NONE',  ( 211.3397459621556038, -90.00000000000007105, 50.00000000000001421 ) ) ;
#5965 = CIRCLE ( 'NONE', #1780, 2.500000000000002220 ) ;
#5966 = ORIENTED_EDGE ( 'NONE', *, *, #531, .F. ) ;
#5967 = EDGE_CURVE ( 'NONE', #140, #2298, #824, .T. ) ;
#5968 = VERTEX_POINT ( 'NONE', #12663 ) ;
#5969 = AXIS2_PLACEMENT_3D ( 'NONE', #11239, #11107, #3353 ) ;
#5970 = ORIENTED_EDGE ( 'NONE', *, *, #14031, .T. ) ;
#5971 = CARTESIAN_POINT ( 'NONE',  ( 347.0000000000000000, 8.660254037844390851, 205.0000000000000284 ) ) ;
#5972 = VECTOR ( 'NONE', #13919, 1000.000000000000000 ) ;
#5973 = AXIS2_PLACEMENT_3D ( 'NONE', #7257, #1733, #5100 ) ;
#5974 = VERTEX_POINT ( 'NONE', #3750 ) ;
#5975 = CARTESIAN_POINT ( 'NONE',  ( 25.00000000000000000, 2.516649172247811061E-16, -2.055000000000000160 ) ) ;
#5976 = EDGE_LOOP ( 'NONE', ( #7846, #10298, #7473, #3221 ) ) ;
#5977 = CARTESIAN_POINT ( 'NONE',  ( 119.9999999999999147, -24.99999999999999289, -19.99999999999998934 ) ) ;
#5978 = CARTESIAN_POINT ( 'NONE',  ( 0.000000000000000000, 0.000000000000000000, -4.484454397937119197 ) ) ;
#5979 = CARTESIAN_POINT ( 'NONE',  ( -145.0000000000000284, -75.00000000000008527, 30.00000000000000000 ) ) ;
#5980 = VECTOR ( 'NONE', #1430, 1000.000000000000114 ) ;
#5981 = PLANE ( 'NONE',  #8370 ) ;
#5982 = CARTESIAN_POINT ( 'NONE',  ( 5.200000000000002842, 3.306546357697854226E-16, 2.700000000000000622 ) ) ;
#5983 = COLOUR_RGB ( '',0.8941176470588234615, 0.8941176470588234615, 0.8941176470588234615 ) ;
#5984 = CARTESIAN_POINT ( 'NONE',  ( 134.9999999999999432, -36.99999999999997868, 10.00000000000000178 ) ) ;
#5985 = EDGE_LOOP ( 'NONE', ( #12016, #13048 ) ) ;
#5986 = EDGE_LOOP ( 'NONE', ( #12619, #12076, #11050, #210 ) ) ;
#5987 =( LENGTH_UNIT ( ) NAMED_UNIT ( * ) SI_UNIT ( .MILLI., .METRE. ) );
#5988 = CARTESIAN_POINT ( 'NONE',  ( 236.4999999999999432, -85.00000000000007105, 190.0000000000000000 ) ) ;
#5989 = DIRECTION ( 'NONE',  ( 0.000000000000000000, 0.000000000000000000, -1.000000000000000000 ) ) ;
#5990 = DIRECTION ( 'NONE',  ( -0.000000000000000000, -1.000000000000000000, -0.000000000000000000 ) ) ;
#5991 = EDGE_CURVE ( 'NONE', #4728, #11362, #7092, .T. ) ;
#5992 = ORIENTED_EDGE ( 'NONE', *, *, #11550, .T. ) ;
#5993 = DIRECTION ( 'NONE',  ( -1.000000000000000000, 0.000000000000000000, 0.000000000000000000 ) ) ;
#5994 = CARTESIAN_POINT ( 'NONE',  ( 4.000000000000000000, 2.309401076758497151, -5.000000000000000000 ) ) ;
#5995 = DIRECTION ( 'NONE',  ( 0.000000000000000000, 0.000000000000000000, 1.000000000000000000 ) ) ;
#5996 = AXIS2_PLACEMENT_3D ( 'NONE', #3788, #335, #11259 ) ;
#5997 = DIRECTION ( 'NONE',  ( 0.000000000000000000, 0.000000000000000000, 1.000000000000000000 ) ) ;
#5998 = ORIENTED_EDGE ( 'NONE', *, *, #7276, .T. ) ;
#5999 = CARTESIAN_POINT ( 'NONE',  ( 25.00000000000000000, 2.055000000000000160, 0.000000000000000000 ) ) ;
#6000 = PRODUCT_DEFINITION_SHAPE ( 'NONE', 'NONE',  #14355 ) ;
#6001 = FACE_OUTER_BOUND ( 'NONE', #9836, .T. ) ;
#6002 = ADVANCED_FACE ( 'NONE', ( #3425 ), #8721, .F. ) ;
#6003 = ORIENTED_EDGE ( 'NONE', *, *, #10557, .T. ) ;
#6004 = DIRECTION ( 'NONE',  ( 0.000000000000000000, 0.000000000000000000, 1.000000000000000000 ) ) ;
#6005 = CARTESIAN_POINT ( 'NONE',  ( 137.3500000000000227, -75.00000000000008527, -186.2999999999999829 ) ) ;
#6006 = CARTESIAN_POINT ( 'NONE',  ( 269.0000000000000000, -8.660254037844389075, 199.9990000000000236 ) ) ;
#6007 = VECTOR ( 'NONE', #12379, 1000.000000000000000 ) ;
#6008 = DIRECTION ( 'NONE',  ( 0.000000000000000000, 0.000000000000000000, -1.000000000000000000 ) ) ;
#6009 = DIRECTION ( 'NONE',  ( 0.000000000000000000, 0.000000000000000000, 1.000000000000000000 ) ) ;
#6010 = FACE_OUTER_BOUND ( 'NONE', #1634, .T. ) ;
#6011 = CARTESIAN_POINT ( 'NONE',  ( 2.682243648011666703, 3.070208061305304881, -0.04852650426601266831 ) ) ;
#6012 = ADVANCED_FACE ( 'NONE', ( #8164 ), #3818, .F. ) ;
#6013 = ITEM_DEFINED_TRANSFORMATION ( 'NONE', 'NONE', #2599,  #14039 ) ;
#6014 = ORIENTED_EDGE ( 'NONE', *, *, #12358, .T. ) ;
#6015 = ORIENTED_EDGE ( 'NONE', *, *, #2069, .T. ) ;
#6016 = CARTESIAN_POINT ( 'NONE',  ( -304.9999999999999432, 45.00000000000001421, 30.00000000000000000 ) ) ;
#6017 = ORIENTED_EDGE ( 'NONE', *, *, #1221, .T. ) ;
#6018 = CARTESIAN_POINT ( 'NONE',  ( 1.411581201560190495E-15, 4.862606272033091592, -3.745885042887436622 ) ) ;
#6019 = CARTESIAN_POINT ( 'NONE',  ( -299.9999999999999432, -75.00000000000008527, 30.00000000000002842 ) ) ;
#6020 = ORIENTED_EDGE ( 'NONE', *, *, #13161, .T. ) ;
#6021 = CARTESIAN_POINT ( 'NONE',  ( 2.500000000000000000, 2.500728763858895382E-16, -2.041999999999999815 ) ) ;
#6022 = ORIENTED_EDGE ( 'NONE', *, *, #2424, .T. ) ;
#6023 = CIRCLE ( 'NONE', #7178, 2.500000000000002220 ) ;
#6024 = DIRECTION ( 'NONE',  ( -1.000000000000000000, 0.000000000000000000, 0.000000000000000000 ) ) ;
#6025 = DIRECTION ( 'NONE',  ( 0.000000000000000000, 0.000000000000000000, -1.000000000000000000 ) ) ;
#6026 = ORIENTED_EDGE ( 'NONE', *, *, #5055, .F. ) ;
#6027 = VECTOR ( 'NONE', #2181, 1000.000000000000000 ) ;
#6028 = FACE_OUTER_BOUND ( 'NONE', #6349, .T. ) ;
#6029 = CARTESIAN_POINT ( 'NONE',  ( -6.473970235329672780E-16, -4.862606272033106691, -3.745885042887442395 ) ) ;
#6030 = SURFACE_SIDE_STYLE ('',( #7046 ) ) ;
#6031 = CARTESIAN_POINT ( 'NONE',  ( 233.9999999999999432, -85.00000000000007105, 190.0000000000000000 ) ) ;
#6032 = EDGE_CURVE ( 'NONE', #486, #2517, #12594, .T. ) ;
#6033 = SHAPE_DEFINITION_REPRESENTATION ( #12484, #3385 ) ;
#6034 = FACE_OUTER_BOUND ( 'NONE', #5747, .T. ) ;
#6035 = ADVANCED_FACE ( 'NONE', ( #3681 ), #8091, .F. ) ;
#6036 = CONICAL_SURFACE ( 'NONE', #11591, 2.500000000000002220, 0.7853981633974521648 ) ;
#6037 = ORIENTED_EDGE ( 'NONE', *, *, #7373, .T. ) ;
#6038 =( REPRESENTATION_RELATIONSHIP ('NONE','NONE', #11251, #208 ) REPRESENTATION_RELATIONSHIP_WITH_TRANSFORMATION ( #3359 )SHAPE_REPRESENTATION_RELATIONSHIP( ) );
#6039 = CIRCLE ( 'NONE', #7187, 10.00000000000000888 ) ;
#6040 = DIRECTION ( 'NONE',  ( 0.000000000000000000, 0.000000000000000000, 1.000000000000000000 ) ) ;
#6041 = ORIENTED_EDGE ( 'NONE', *, *, #11728, .F. ) ;
#6042 = VECTOR ( 'NONE', #9129, 1000.000000000000000 ) ;
#6043 = DIRECTION ( 'NONE',  ( -1.000000000000000000, -0.000000000000000000, -0.000000000000000000 ) ) ;
#6044 = VERTEX_POINT ( 'NONE', #4989 ) ;
#6045 = PLANE ( 'NONE',  #5042 ) ;
#6046 = EDGE_LOOP ( 'NONE', ( #5206, #572 ) ) ;
#6047 = DIRECTION ( 'NONE',  ( 0.000000000000000000, 0.000000000000000000, 1.000000000000000000 ) ) ;
#6048 = EDGE_CURVE ( 'NONE', #8647, #898, #1757, .T. ) ;
#6049 = VECTOR ( 'NONE', #13178, 1000.000000000000000 ) ;
#6050 = CARTESIAN_POINT ( 'NONE',  ( 137.3500000000000227, -75.00000000000008527, -190.0000000000000000 ) ) ;
#6051 = CARTESIAN_POINT ( 'NONE',  ( 2.500000000000000000, 1.178949249685212974, -2.042000000000001148 ) ) ;
#6052 = DIRECTION ( 'NONE',  ( 1.000000000000000000, 0.000000000000000000, 0.000000000000000000 ) ) ;
#6053 = ADVANCED_FACE ( 'NONE', ( #303 ), #9407, .F. ) ;
#6054 = DIRECTION ( 'NONE',  ( 1.000000000000000000, 0.000000000000000000, 0.000000000000000000 ) ) ;
#6055 = ORIENTED_EDGE ( 'NONE', *, *, #8992, .F. ) ;
#6056 = ORIENTED_EDGE ( 'NONE', *, *, #6068, .T. ) ;
#6057 = AXIS2_PLACEMENT_3D ( 'NONE', #7927, #12366, #4606 ) ;
#6058 = ORIENTED_EDGE ( 'NONE', *, *, #8926, .T. ) ;
#6059 = DIRECTION ( 'NONE',  ( 1.000000000000000000, 0.000000000000000000, 0.000000000000000000 ) ) ;
#6060 = DIRECTION ( 'NONE',  ( -0.000000000000000000, -0.000000000000000000, 1.000000000000000000 ) ) ;
#6061 = EDGE_CURVE ( 'NONE', #13881, #649, #7325, .T. ) ;
#6062 = DIRECTION ( 'NONE',  ( 0.000000000000000000, -0.000000000000000000, 1.000000000000000000 ) ) ;
#6063 = ORIENTED_EDGE ( 'NONE', *, *, #8900, .F. ) ;
#6064 = EDGE_CURVE ( 'NONE', #2741, #5325, #8483, .T. ) ;
#6065 = CIRCLE ( 'NONE', #10717, 12.44999999999999929 ) ;
#6066 = FACE_OUTER_BOUND ( 'NONE', #5854, .T. ) ;
#6067 = AXIS2_PLACEMENT_3D ( 'NONE', #10351, #9348, #11587 ) ;
#6068 = EDGE_CURVE ( 'NONE', #7334, #7167, #8231, .T. ) ;
#6069 = CYLINDRICAL_SURFACE ( 'NONE', #11130, 2.649999999999985700 ) ;
#6070 = DIRECTION ( 'NONE',  ( 0.000000000000000000, 0.000000000000000000, -1.000000000000000000 ) ) ;
#6071 = DIRECTION ( 'NONE',  ( -0.000000000000000000, 0.000000000000000000, 1.000000000000000000 ) ) ;
#6072 = DIRECTION ( 'NONE',  ( -0.000000000000000000, -0.000000000000000000, 1.000000000000000000 ) ) ;
#6073 = ORIENTED_EDGE ( 'NONE', *, *, #2581, .F. ) ;
#6074 = DIRECTION ( 'NONE',  ( -0.000000000000000000, 1.000000000000000000, -0.000000000000000000 ) ) ;
#6075 = TOROIDAL_SURFACE ( 'NONE', #9089, 2.700000000000000178, 0.2000000000000000111 ) ;
#6076 = CARTESIAN_POINT ( 'NONE',  ( 0.2500000000000002220, 0.000000000000000000, 0.000000000000000000 ) ) ;
#6077 = AXIS2_PLACEMENT_3D ( 'NONE', #7976, #2485, #7844 ) ;
#6078 = ORIENTED_EDGE ( 'NONE', *, *, #2777, .F. ) ;
#6079 = DIRECTION ( 'NONE',  ( -1.000000000000000000, -0.000000000000000000, -0.000000000000000000 ) ) ;
#6080 = DIRECTION ( 'NONE',  ( 0.000000000000000000, 0.000000000000000000, 1.000000000000000000 ) ) ;
#6081 = CARTESIAN_POINT ( 'NONE',  ( 2.500000000000000444, 0.000000000000000000, -5.000000000000000888 ) ) ;
#6082 = DIRECTION ( 'NONE',  ( 1.000000000000000000, 0.000000000000000000, 0.000000000000000000 ) ) ;
#6083 = CARTESIAN_POINT ( 'NONE',  ( 2.740000000000000213, -0.9838866223905674557, -0.5150000000000000133 ) ) ;
#6084 =( NAMED_UNIT ( * ) SI_UNIT ( $, .STERADIAN. ) SOLID_ANGLE_UNIT ( ) );
#6085 = AXIS2_PLACEMENT_3D ( 'NONE', #7645, #5340, #8669 ) ;
#6086 = CARTESIAN_POINT ( 'NONE',  ( -2.807080416178626692, 3.225969019225154444, -3.502507215260441065 ) ) ;
#6087 = CARTESIAN_POINT ( 'NONE',  ( 0.2277608394786177770, 1.419059478511995659E-15, -10.72500000000000142 ) ) ;
#6088 = MECHANICAL_DESIGN_GEOMETRIC_PRESENTATION_REPRESENTATION (  '', ( #12571 ), #7448 ) ;
#6089 = ADVANCED_FACE ( 'NONE', ( #10021 ), #2255, .T. ) ;
#6090 = EDGE_LOOP ( 'NONE', ( #696, #8694, #10235, #8014 ) ) ;
#6091 = CARTESIAN_POINT ( 'NONE',  ( 181.0000000000000000, 8.660254037844390851, 199.9990000000000236 ) ) ;
#6092 = ORIENTED_EDGE ( 'NONE', *, *, #2241, .T. ) ;
#6093 = DIRECTION ( 'NONE',  ( 1.000000000000000000, 0.000000000000000000, 0.000000000000000000 ) ) ;
#6094 = DIRECTION ( 'NONE',  ( -1.000000000000000000, 0.000000000000000000, 0.000000000000000000 ) ) ;
#6095 = CIRCLE ( 'NONE', #11894, 0.5155456020628804703 ) ;
#6096 = APPLICATION_CONTEXT ( 'automotive_design' ) ;
#6097 = ORIENTED_EDGE ( 'NONE', *, *, #9936, .F. ) ;
#6098 = CARTESIAN_POINT ( 'NONE',  ( -4.204015924366189871, 1.626724848190922446, -3.610627190413390419 ) ) ;
#6099 = VERTEX_POINT ( 'NONE', #5921 ) ;
#6100 = DIRECTION ( 'NONE',  ( -0.000000000000000000, -0.000000000000000000, 1.000000000000000000 ) ) ;
#6101 = CYLINDRICAL_SURFACE ( 'NONE', #13601, 4.250000000000000000 ) ;
#6102 = ORIENTED_EDGE ( 'NONE', *, *, #13724, .T. ) ;
#6103 = DIRECTION ( 'NONE',  ( 1.000000000000000000, 9.912705577010325549E-17, 0.000000000000000000 ) ) ;
#6104 = DIRECTION ( 'NONE',  ( 0.000000000000000000, 0.000000000000000000, -1.000000000000000000 ) ) ;
#6105 = SURFACE_STYLE_USAGE ( .BOTH. , #1669 ) ;
#6106 = ITEM_DEFINED_TRANSFORMATION ( 'NONE', 'NONE', #3746,  #14039 ) ;
#6107 = CARTESIAN_POINT ( 'NONE',  ( 0.000000000000000000, 0.000000000000000000, 0.000000000000000000 ) ) ;
#6108 = ADVANCED_FACE ( 'NONE', ( #11510 ), #4508, .F. ) ;
#6109 = VERTEX_POINT ( 'NONE', #2812 ) ;
#6110 = ORIENTED_EDGE ( 'NONE', *, *, #5694, .T. ) ;
#6111 = CARTESIAN_POINT ( 'NONE',  ( 28.70000000000000284, 0.000000000000000000, 0.000000000000000000 ) ) ;
#6112 = VERTEX_POINT ( 'NONE', #5070 ) ;
#6113 = CARTESIAN_POINT ( 'NONE',  ( 386.6666666666666288, -25.00000000000000000, 225.1500000000000625 ) ) ;
#6114 = ORIENTED_EDGE ( 'NONE', *, *, #6715, .F. ) ;
#6115 = CYLINDRICAL_SURFACE ( 'NONE', #11283, 2.500000000000002220 ) ;
#6116 = EDGE_LOOP ( 'NONE', ( #11970, #5317, #11756 ) ) ;
#6117 = EDGE_CURVE ( 'NONE', #840, #13282, #6139, .T. ) ;
#6118 = LINE ( 'NONE', #7134, #6426 ) ;
#6119 = EDGE_CURVE ( 'NONE', #13937, #2529, #10570, .T. ) ;
#6120 = CARTESIAN_POINT ( 'NONE',  ( -30.00000000000002842, -225.0000000000000000, -190.0000000000000000 ) ) ;
#6121 = CARTESIAN_POINT ( 'NONE',  ( 1.391697335622810172, 4.043246145443375461, -3.503898532754365913 ) ) ;
#6122 = CARTESIAN_POINT ( 'NONE',  ( 302.5000000000000000, -56.99999999999997158, -169.9999999999999716 ) ) ;
#6123 = CYLINDRICAL_SURFACE ( 'NONE', #12305, 20.00000000000000000 ) ;
#6124 = CARTESIAN_POINT ( 'NONE',  ( 224.9999999999999716, -85.00000000000007105, 0.000000000000000000 ) ) ;
#6125 = PRODUCT_DEFINITION_SHAPE ( 'NONE', 'NONE',  #14344 ) ;
#6126 = ORIENTED_EDGE ( 'NONE', *, *, #11435, .F. ) ;
#6127 = EDGE_LOOP ( 'NONE', ( #12285, #3154, #4677, #9672 ) ) ;
#6128 = CARTESIAN_POINT ( 'NONE',  ( 222.4999999999999147, -85.00000000000009948, -17.55500000000000327 ) ) ;
#6129 = EDGE_LOOP ( 'NONE', ( #12707, #9544, #2444, #4866 ) ) ;
#6130 = CARTESIAN_POINT ( 'NONE',  ( 134.9999999999999432, -56.99999999999997158, -180.0000000000000000 ) ) ;
#6131 = ADVANCED_FACE ( 'NONE', ( #9480 ), #7228, .T. ) ;
#6132 = DIRECTION ( 'NONE',  ( 0.000000000000000000, 0.000000000000000000, 1.000000000000000000 ) ) ;
#6133 = CARTESIAN_POINT ( 'NONE',  ( 5.200000000000002842, 0.000000000000000000, 0.000000000000000000 ) ) ;
#6134 = ORIENTED_EDGE ( 'NONE', *, *, #3325, .T. ) ;
#6135 = LINE ( 'NONE', #522, #13685 ) ;
#6136 = DIRECTION ( 'NONE',  ( -1.000000000000000000, -0.000000000000000000, -0.000000000000000000 ) ) ;
#6137 = DIRECTION ( 'NONE',  ( -1.000000000000000000, 0.000000000000000000, 0.000000000000000000 ) ) ;
#6138 = CARTESIAN_POINT ( 'NONE',  ( 2.740000000000000213, 0.9838866223910001096, -0.5150000000000001243 ) ) ;
#6139 = LINE ( 'NONE', #1707, #4321 ) ;
#6140 = EDGE_CURVE ( 'NONE', #9211, #8841, #3172, .T. ) ;
#6141 = ADVANCED_FACE ( 'NONE', ( #3356 ), #12054, .T. ) ;
#6142 = AXIS2_PLACEMENT_3D ( 'NONE', #12438, #4757, #7996 ) ;
#6143 = ADVANCED_FACE ( 'NONE', ( #9872 ), #7564, .F. ) ;
#6144 = EDGE_CURVE ( 'NONE', #9739, #5872, #108, .T. ) ;
#6145 = ORIENTED_EDGE ( 'NONE', *, *, #2511, .F. ) ;
#6146 = LINE ( 'NONE', #3684, #4872 ) ;
#6147 = PLANE ( 'NONE',  #9041 ) ;
#6148 = EDGE_LOOP ( 'NONE', ( #1595, #4983 ) ) ;
#6149 = FACE_OUTER_BOUND ( 'NONE', #2263, .T. ) ;
#6150 = AXIS2_PLACEMENT_3D ( 'NONE', #8266, #11682, #405 ) ;
#6151 = DIRECTION ( 'NONE',  ( 1.000000000000000000, 0.000000000000000000, 0.000000000000000000 ) ) ;
#6152 = AXIS2_PLACEMENT_3D ( 'NONE', #172, #3345, #3607 ) ;
#6153 = DIRECTION ( 'NONE',  ( -0.7071067811865364705, 8.659560562355067211E-17, -0.7071067811865584529 ) ) ;
#6154 = CARTESIAN_POINT ( 'NONE',  ( -4.000000000000000000, 2.309401076758498483, -0.4999999999999927280 ) ) ;
#6155 = FACE_OUTER_BOUND ( 'NONE', #11082, .T. ) ;
#6156 = CARTESIAN_POINT ( 'NONE',  ( -0.5469614295416921346, 4.303013824936271270, -3.535263753543735454 ) ) ;
#6157 = CONTEXT_DEPENDENT_SHAPE_REPRESENTATION ( #2521, #4045 ) ;
#6158 = ORIENTED_EDGE ( 'NONE', *, *, #14212, .F. ) ;
#6159 = PLANE ( 'NONE',  #4061 ) ;
#6160 = AXIS2_PLACEMENT_3D ( 'NONE', #180, #4637, #2174 ) ;
#6161 = ORIENTED_EDGE ( 'NONE', *, *, #10859, .T. ) ;
#6162 = DIRECTION ( 'NONE',  ( 0.000000000000000000, -1.000000000000000000, 0.000000000000000000 ) ) ;
#6163 = DIRECTION ( 'NONE',  ( -0.9396926207859138680, 0.000000000000000000, -0.3420201433256536139 ) ) ;
#6164 = EDGE_LOOP ( 'NONE', ( #2961, #3431 ) ) ;
#6165 = DIRECTION ( 'NONE',  ( -0.000000000000000000, -0.000000000000000000, 1.000000000000000000 ) ) ;
#6166 = ORIENTED_EDGE ( 'NONE', *, *, #3754, .F. ) ;
#6167 = LINE ( 'NONE', #12622, #5242 ) ;
#6168 = CARTESIAN_POINT ( 'NONE',  ( 137.3500000000000227, -75.00000000000008527, 190.0000000000000000 ) ) ;
#6169 = ORIENTED_EDGE ( 'NONE', *, *, #1553, .T. ) ;
#6170 = CIRCLE ( 'NONE', #12420, 2.649999999999985700 ) ;
#6171 = CARTESIAN_POINT ( 'NONE',  ( 140.0000000000000000, -75.00000000000008527, 190.0000000000000000 ) ) ;
#6172 = EDGE_CURVE ( 'NONE', #8606, #6112, #3405, .T. ) ;
#6173 = FACE_OUTER_BOUND ( 'NONE', #8420, .T. ) ;
#6174 = AXIS2_PLACEMENT_3D ( 'NONE', #3260, #7662, #12097 ) ;
#6175 = PRODUCT_CONTEXT ( 'NONE', #10266, 'mechanical' ) ;
#6176 = DIRECTION ( 'NONE',  ( 0.000000000000000000, 0.000000000000000000, -1.000000000000000000 ) ) ;
#6177 = EDGE_LOOP ( 'NONE', ( #9451, #9774, #261, #6911 ) ) ;
#6178 = EDGE_LOOP ( 'NONE', ( #755, #1968, #8335 ) ) ;
#6179 = ORIENTED_EDGE ( 'NONE', *, *, #1576, .T. ) ;
#6180 = AXIS2_PLACEMENT_3D ( 'NONE', #2457, #11385, #6882 ) ;
#6181 = ORIENTED_EDGE ( 'NONE', *, *, #3069, .F. ) ;
#6182 = DIRECTION ( 'NONE',  ( 1.000000000000000000, 0.000000000000000000, -0.000000000000000000 ) ) ;
#6183 = AXIS2_PLACEMENT_3D ( 'NONE', #6799, #9113, #11224 ) ;
#6184 = ORIENTED_EDGE ( 'NONE', *, *, #4592, .T. ) ;
#6185 = DIRECTION ( 'NONE',  ( 0.000000000000000000, 0.000000000000000000, 1.000000000000000000 ) ) ;
#6186 = ORIENTED_EDGE ( 'NONE', *, *, #6640, .T. ) ;
#6187 = CARTESIAN_POINT ( 'NONE',  ( 299.9999999999999432, -95.00000000000008527, -190.0000000000000000 ) ) ;
#6188 = AXIS2_PLACEMENT_3D ( 'NONE', #12131, #1229, #11190 ) ;
#6189 = UNCERTAINTY_MEASURE_WITH_UNIT (LENGTH_MEASURE( 1.000000000000000082E-05 ), #13673, 'distance_accuracy_value', 'NONE');
#6190 = AXIS2_PLACEMENT_3D ( 'NONE', #1976, #8509, #7558 ) ;
#6191 = CARTESIAN_POINT ( 'NONE',  ( 137.6499999999999773, 45.00000000000001421, -1.230770033143087371E-15 ) ) ;
#6192 = FACE_BOUND ( 'NONE', #7484, .T. ) ;
#6193 = VECTOR ( 'NONE', #8806, 1000.000000000000000 ) ;
#6194 = LINE ( 'NONE', #12053, #6761 ) ;
#6195 = CARTESIAN_POINT ( 'NONE',  ( 4.999999999999999112, 0.000000000000000000, 200.0000000000000000 ) ) ;
#6196 = AXIS2_PLACEMENT_3D ( 'NONE', #1956, #3278, #7680 ) ;
#6197 = DIRECTION ( 'NONE',  ( 0.000000000000000000, 0.000000000000000000, -1.000000000000000000 ) ) ;
#6198 = EDGE_LOOP ( 'NONE', ( #8683, #7258, #12979, #13330 ) ) ;
#6199 = EDGE_CURVE ( 'NONE', #5408, #2276, #13407, .T. ) ;
#6200 = AXIS2_PLACEMENT_3D ( 'NONE', #11902, #12766, #554 ) ;
#6201 = ORIENTED_EDGE ( 'NONE', *, *, #11650, .F. ) ;
#6202 = AXIS2_PLACEMENT_3D ( 'NONE', #6673, #3208, #4568 ) ;
#6203 = CARTESIAN_POINT ( 'NONE',  ( -20.63749999999999929, 0.000000000000000000, 0.000000000000000000 ) ) ;
#6204 = CIRCLE ( 'NONE', #4355, 5.000000000000004441 ) ;
#6205 = DIRECTION ( 'NONE',  ( 1.000000000000000000, 0.000000000000000000, 0.000000000000000000 ) ) ;
#6206 = CARTESIAN_POINT ( 'NONE',  ( 305.0000000000000000, -36.99999999999997868, -169.9999999999999716 ) ) ;
#6207 = FACE_BOUND ( 'NONE', #11539, .T. ) ;
#6208 = VERTEX_POINT ( 'NONE', #3281 ) ;
#6209 = CIRCLE ( 'NONE', #4598, 2.649999999999985700 ) ;
#6210 = DIRECTION ( 'NONE',  ( 1.000000000000000000, 0.000000000000000000, -0.000000000000000000 ) ) ;
#6211 = CARTESIAN_POINT ( 'NONE',  ( 144.9999999999999716, -64.99999999999997158, 0.000000000000000000 ) ) ;
#6212 = CARTESIAN_POINT ( 'NONE',  ( 140.0000000000000000, -95.00000000000008527, -190.0000000000000000 ) ) ;
#6213 = CARTESIAN_POINT ( 'NONE',  ( 134.9999999999999716, 45.00000000000001421, -1.230770033143087371E-15 ) ) ;
#6214 = EDGE_CURVE ( 'NONE', #5872, #8099, #4366, .T. ) ;
#6215 = VERTEX_POINT ( 'NONE', #11111 ) ;
#6216 = AXIS2_PLACEMENT_3D ( 'NONE', #6990, #11421, #3588 ) ;
#6217 = CARTESIAN_POINT ( 'NONE',  ( 136.6666666666666288, -14.99999999999999822, 222.5000000000000853 ) ) ;
#6218 = VECTOR ( 'NONE', #10930, 1000.000000000000000 ) ;
#6219 = CARTESIAN_POINT ( 'NONE',  ( 53.33333333333330017, -20.00000000000000000, -222.5000000000000853 ) ) ;
#6220 = ORIENTED_EDGE ( 'NONE', *, *, #11262, .F. ) ;
#6221 = LINE ( 'NONE', #10654, #3624 ) ;
#6222 = EDGE_CURVE ( 'NONE', #8495, #7265, #10819, .T. ) ;
#6223 = ADVANCED_FACE ( 'NONE', ( #2180 ), #1068, .F. ) ;
#6224 =( REPRESENTATION_RELATIONSHIP ('NONE','NONE', #11251, #4229 ) REPRESENTATION_RELATIONSHIP_WITH_TRANSFORMATION ( #318 )SHAPE_REPRESENTATION_RELATIONSHIP( ) );
#6225 = CARTESIAN_POINT ( 'NONE',  ( 1.794155980045911036, 0.000000000000000000, 0.000000000000000000 ) ) ;
#6226 = AXIS2_PLACEMENT_3D ( 'NONE', #5539, #12280, #9825 ) ;
#6227 = DIRECTION ( 'NONE',  ( -0.000000000000000000, -0.000000000000000000, -1.000000000000000000 ) ) ;
#6228 = DIRECTION ( 'NONE',  ( 0.000000000000000000, 1.000000000000000000, 0.000000000000000000 ) ) ;
#6229 = CARTESIAN_POINT ( 'NONE',  ( 0.02448733951239481094, 4.877042772274728044, -3.751161874094022242 ) ) ;
#6230 = CIRCLE ( 'NONE', #13867, 0.8509999999999999787 ) ;
#6231 = ADVANCED_FACE ( 'NONE', ( #9947 ), #5175, .F. ) ;
#6232 = CONTEXT_DEPENDENT_SHAPE_REPRESENTATION ( #8240, #7401 ) ;
#6233 = ORIENTED_EDGE ( 'NONE', *, *, #10110, .F. ) ;
#6234 = DIRECTION ( 'NONE',  ( 1.000000000000000000, 0.000000000000000000, 0.000000000000000000 ) ) ;
#6235 = ORIENTED_EDGE ( 'NONE', *, *, #3787, .F. ) ;
#6236 = LINE ( 'NONE', #143, #4254 ) ;
#6237 = DIRECTION ( 'NONE',  ( 0.000000000000000000, -0.5000000000000012212, -0.8660254037844380415 ) ) ;
#6238 = VERTEX_POINT ( 'NONE', #47 ) ;
#6239 = DIRECTION ( 'NONE',  ( 0.000000000000000000, 1.000000000000000000, 1.153406566473941260E-16 ) ) ;
#6240 = EDGE_LOOP ( 'NONE', ( #3549, #4274, #12865, #437 ) ) ;
#6241 = DIRECTION ( 'NONE',  ( -0.000000000000000000, -0.000000000000000000, -1.000000000000000000 ) ) ;
#6242 = ADVANCED_FACE ( 'NONE', ( #4573 ), #3422, .F. ) ;
#6243 = DIRECTION ( 'NONE',  ( 1.000000000000000000, 0.000000000000000000, 0.000000000000000000 ) ) ;
#6244 = ORIENTED_EDGE ( 'NONE', *, *, #977, .T. ) ;
#6245 = ADVANCED_FACE ( 'NONE', ( #8853 ), #10971, .F. ) ;
#6246 = CARTESIAN_POINT ( 'NONE',  ( 1.999999999999998668, 0.000000000000000000, -10.20000000000000107 ) ) ;
#6247 = FACE_OUTER_BOUND ( 'NONE', #12982, .T. ) ;
#6248 = EDGE_CURVE ( 'NONE', #1243, #9474, #8991, .T. ) ;
#6249 = ITEM_DEFINED_TRANSFORMATION ( 'NONE', 'NONE', #3311,  #14039 ) ;
#6250 = LINE ( 'NONE', #10683, #616 ) ;
#6251 = ORIENTED_EDGE ( 'NONE', *, *, #13379, .T. ) ;
#6252 = AXIS2_PLACEMENT_3D ( 'NONE', #7859, #6789, #12437 ) ;
#6253 = EDGE_LOOP ( 'NONE', ( #11118, #12440, #7626, #4032 ) ) ;
#6254 = DIRECTION ( 'NONE',  ( -1.000000000000000000, 0.000000000000000000, 0.000000000000000000 ) ) ;
#6255 = VERTEX_POINT ( 'NONE', #7888 ) ;
#6256 = CARTESIAN_POINT ( 'NONE',  ( -219.9999999999999147, -85.00000000000009948, 40.00000000000000000 ) ) ;
#6257 = ORIENTED_EDGE ( 'NONE', *, *, #12593, .F. ) ;
#6258 = CARTESIAN_POINT ( 'NONE',  ( 0.2500000000000002220, 4.898587196589412829E-16, -4.000000000000000000 ) ) ;
#6259 = ORIENTED_EDGE ( 'NONE', *, *, #3043, .F. ) ;
#6260 = CARTESIAN_POINT ( 'NONE',  ( 233.9999999999999432, -85.00000000000007105, 190.0000000000000000 ) ) ;
#6261 = DIRECTION ( 'NONE',  ( -0.000000000000000000, 1.000000000000000000, -0.000000000000000000 ) ) ;
#6262 = DIRECTION ( 'NONE',  ( 0.8949343913984706411, 1.487067055422294855E-15, -0.4461977533473793223 ) ) ;
#6263 = CARTESIAN_POINT ( 'NONE',  ( 297.3499999999999659, -95.00000000000008527, 169.9999999999999716 ) ) ;
#6264 = VECTOR ( 'NONE', #421, 1000.000000000000114 ) ;
#6265 = FILL_AREA_STYLE ('',( #10629 ) ) ;
#6266 = PLANE ( 'NONE',  #2287 ) ;
#6267 = ORIENTED_EDGE ( 'NONE', *, *, #12357, .F. ) ;
#6268 = AXIS2_PLACEMENT_3D ( 'NONE', #11143, #4684, #12148 ) ;
#6269 = ORIENTED_EDGE ( 'NONE', *, *, #13228, .T. ) ;
#6270 = EDGE_CURVE ( 'NONE', #6471, #568, #12328, .T. ) ;
#6271 = CARTESIAN_POINT ( 'NONE',  ( 219.9999999999999716, -20.00000000000000000, 222.5000000000000853 ) ) ;
#6272 = CIRCLE ( 'NONE', #12760, 10.00000000000000000 ) ;
#6273 = DIRECTION ( 'NONE',  ( -0.000000000000000000, 1.000000000000000000, -0.000000000000000000 ) ) ;
#6274 = DIRECTION ( 'NONE',  ( 0.000000000000000000, -0.8660254037844390407, -0.4999999999999994449 ) ) ;
#6275 = FACE_BOUND ( 'NONE', #4251, .T. ) ;
#6276 = ORIENTED_EDGE ( 'NONE', *, *, #9528, .F. ) ;
#6277 = LINE ( 'NONE', #5280, #5590 ) ;
#6278 = DIRECTION ( 'NONE',  ( 0.000000000000000000, 1.000000000000000000, 0.000000000000000000 ) ) ;
#6279 = CARTESIAN_POINT ( 'NONE',  ( 0.000000000000000000, 0.000000000000000000, 169.9999999999999716 ) ) ;
#6280 = VECTOR ( 'NONE', #4403, 1000.000000000000000 ) ;
#6281 = CARTESIAN_POINT ( 'NONE',  ( 303.3333333333333144, -25.00000000000000000, 219.8500000000001080 ) ) ;
#6282 = VERTEX_POINT ( 'NONE', #4647 ) ;
#6283 = EDGE_LOOP ( 'NONE', ( #9335, #10813, #11356, #4817 ) ) ;
#6284 = FACE_OUTER_BOUND ( 'NONE', #11747, .T. ) ;
#6285 = PLANE ( 'NONE',  #4197 ) ;
#6286 = AXIS2_PLACEMENT_3D ( 'NONE', #13335, #9203, #3555 ) ;
#6287 = ORIENTED_EDGE ( 'NONE', *, *, #11567, .F. ) ;
#6289 = EDGE_CURVE ( 'NONE', #298, #4150, #5019, .T. ) ;
#6288 = CARTESIAN_POINT ( 'NONE',  ( 470.0000000000000000, -20.00000000000000000, -250.0000000000000000 ) ) ;
#6290 = PRODUCT_DEFINITION_CONTEXT ( 'detailed design', #8311, 'design' ) ;
#6291 = DIRECTION ( 'NONE',  ( 0.000000000000000000, 0.000000000000000000, 1.000000000000000000 ) ) ;
#6292 = EDGE_CURVE ( 'NONE', #7212, #7915, #7105, .T. ) ;
#6293 = UNCERTAINTY_MEASURE_WITH_UNIT (LENGTH_MEASURE( 1.000000000000000082E-05 ), #4002, 'distance_accuracy_value', 'NONE');
#6294 = CYLINDRICAL_SURFACE ( 'NONE', #9179, 5.500000000000005329 ) ;
#6295 = B_SPLINE_CURVE_WITH_KNOTS ( 'NONE', 3,
 ( #12202, #9889, #13290, #126, #60 ),
 .UNSPECIFIED., .F., .F.,
 ( 4, 1, 4 ),
 ( 0.000000000000000000, 0.002309401076758505790, 0.004618802153517011580 ),
 .UNSPECIFIED. ) ;
#6296 = CARTESIAN_POINT ( 'NONE',  ( 303.3333333333333144, -20.00000000000000000, -219.8500000000001080 ) ) ;
#6297 = DIRECTION ( 'NONE',  ( -1.000000000000000000, 0.000000000000000000, 0.000000000000000000 ) ) ;
#6298 =( NAMED_UNIT ( * ) PLANE_ANGLE_UNIT ( ) SI_UNIT ( $, .RADIAN. ) );
#6299 = AXIS2_PLACEMENT_3D ( 'NONE', #11793, #2730, #13963 ) ;
#6300 = B_SPLINE_CURVE_WITH_KNOTS ( 'NONE', 3,
 ( #10178, #4601, #3777, #12615, #9017, #2683 ),
 .UNSPECIFIED., .F., .F.,
 ( 4, 2, 4 ),
 ( 4.336808689942017736E-19, 0.0002095117440864781224, 0.0004190234881729558111 ),
 .UNSPECIFIED. ) ;
#6301 = ORIENTED_EDGE ( 'NONE', *, *, #11515, .F. ) ;
#6302 = EDGE_CURVE ( 'NONE', #1400, #8555, #8496, .T. ) ;
#6303 = DIRECTION ( 'NONE',  ( 0.000000000000000000, 0.000000000000000000, -1.000000000000000000 ) ) ;
#6304 = AXIS2_PLACEMENT_3D ( 'NONE', #4918, #6864, #5850 ) ;
#6305 = EDGE_LOOP ( 'NONE', ( #11992, #4067, #5998, #12317 ) ) ;
#6306 = VECTOR ( 'NONE', #7417, 1000.000000000000000 ) ;
#6307 = DIRECTION ( 'NONE',  ( 1.000000000000000000, 0.000000000000000000, 0.000000000000000000 ) ) ;
#6308 = DIRECTION ( 'NONE',  ( -0.7071067811865502373, 8.659560562354966138E-17, 0.7071067811865447972 ) ) ;
#6309 = VERTEX_POINT ( 'NONE', #8246 ) ;
#6310 = CARTESIAN_POINT ( 'NONE',  ( -4.000000000000000000, -2.309401076758512694, -5.000000000000000000 ) ) ;
#6311 = ORIENTED_EDGE ( 'NONE', *, *, #12885, .F. ) ;
#6313 = EDGE_CURVE ( 'NONE', #12966, #7287, #543, .T. ) ;
#6312 = FACE_OUTER_BOUND ( 'NONE', #9191, .T. ) ;
#6314 = PRODUCT_DEFINITION ( 'UNKNOWN', '', #9808, #3039 ) ;
#6315 = CARTESIAN_POINT ( 'NONE',  ( 93.00000000000000000, -8.660254037844389075, 205.0000000000000284 ) ) ;
#6317 = ORIENTED_EDGE ( 'NONE', *, *, #3580, .F. ) ;
#6316 = AXIS2_PLACEMENT_3D ( 'NONE', #6206, #2947, #11719 ) ;
#6318 = DIRECTION ( 'NONE',  ( -0.000000000000000000, -0.000000000000000000, -1.000000000000000000 ) ) ;
#6319 = CARTESIAN_POINT ( 'NONE',  ( 357.0000000000000000, 8.660254037844390851, 199.9990000000000236 ) ) ;
#6320 = PRODUCT_DEFINITION_FORMATION_WITH_SPECIFIED_SOURCE ( 'ANY', '', #4382, .NOT_KNOWN. ) ;
#6321 = PRESENTATION_STYLE_ASSIGNMENT (( #1817 ) ) ;
#6322 = PRESENTATION_LAYER_ASSIGNMENT (  '', '', ( #12571 ) ) ;
#6323 = ADVANCED_FACE ( 'NONE', ( #5001 ), #8176, .F. ) ;
#6324 = AXIS2_PLACEMENT_3D ( 'NONE', #3841, #8257, #13916 ) ;
#6325 = CARTESIAN_POINT ( 'NONE',  ( 203.5000000000000000, -85.00000000000007105, 190.0000000000000000 ) ) ;
#6326 = CONTEXT_DEPENDENT_SHAPE_REPRESENTATION ( #2867, #8768 ) ;
#6327 = CARTESIAN_POINT ( 'NONE',  ( -4.000000000000000000, 1.700094919196744270, -3.320312364301766017 ) ) ;
#6328 = ORIENTED_EDGE ( 'NONE', *, *, #13997, .T. ) ;
#6329 = ORIENTED_EDGE ( 'NONE', *, *, #3964, .F. ) ;
#6330 = ADVANCED_FACE ( 'NONE', ( #3556 ), #7336, .F. ) ;
#6331 = EDGE_CURVE ( 'NONE', #2838, #3406, #8032, .T. ) ;
#6332 = DIRECTION ( 'NONE',  ( -0.000000000000000000, 0.000000000000000000, 1.000000000000000000 ) ) ;
#6333 = CIRCLE ( 'NONE', #12340, 2.700000000000000622 ) ;
#6334 = ORIENTED_EDGE ( 'NONE', *, *, #9790, .F. ) ;
#6335 = EDGE_CURVE ( 'NONE', #10867, #2928, #4332, .T. ) ;
#6336 = EDGE_CURVE ( 'NONE', #12884, #12902, #9187, .T. ) ;
#6337 = CARTESIAN_POINT ( 'NONE',  ( 3.700000000000000178, 2.500000000000000000, 0.000000000000000000 ) ) ;
#6338 = VERTEX_POINT ( 'NONE', #391 ) ;
#6339 = ORIENTED_EDGE ( 'NONE', *, *, #8451, .T. ) ;
#6340 = FACE_OUTER_BOUND ( 'NONE', #1936, .T. ) ;
#6341 = ORIENTED_EDGE ( 'NONE', *, *, #10658, .T. ) ;
#6342 = DIRECTION ( 'NONE',  ( -0.000000000000000000, -0.000000000000000000, 1.000000000000000000 ) ) ;
#6343 = EDGE_CURVE ( 'NONE', #6309, #8482, #12471, .T. ) ;
#6344 = UNCERTAINTY_MEASURE_WITH_UNIT (LENGTH_MEASURE( 1.000000000000000082E-05 ), #6635, 'distance_accuracy_value', 'NONE');
#6345 = PLANE ( 'NONE',  #6190 ) ;
#6346 = LINE ( 'NONE', #1919, #9190 ) ;
#6347 = DIRECTION ( 'NONE',  ( 0.000000000000000000, 0.000000000000000000, 1.000000000000000000 ) ) ;
#6348 = DIRECTION ( 'NONE',  ( -0.000000000000000000, -0.000000000000000000, -1.000000000000000000 ) ) ;
#6349 = EDGE_LOOP ( 'NONE', ( #2926, #7079, #36, #13544 ) ) ;
#6350 = ORIENTED_EDGE ( 'NONE', *, *, #1413, .F. ) ;
#6351 = CARTESIAN_POINT ( 'NONE',  ( 82.99999999999998579, 8.660254037844390851, 205.0000000000000284 ) ) ;
#6352 = DIRECTION ( 'NONE',  ( -0.000000000000000000, 0.000000000000000000, -1.000000000000000000 ) ) ;
#6353 = FACE_OUTER_BOUND ( 'NONE', #2119, .T. ) ;
#6354 = FACE_BOUND ( 'NONE', #8517, .T. ) ;
#6355 = ORIENTED_EDGE ( 'NONE', *, *, #12301, .T. ) ;
#6356 = LINE ( 'NONE', #12815, #4207 ) ;
#6357 = EDGE_CURVE ( 'NONE', #930, #3366, #7956, .T. ) ;
#6358 = DIRECTION ( 'NONE',  ( 0.8949343913984706411, -0.4461977533473793778, 0.000000000000000000 ) ) ;
#6359 = DIRECTION ( 'NONE',  ( 1.000000000000000000, 0.000000000000000000, 6.123233995736766036E-17 ) ) ;
#6360 = LINE ( 'NONE', #2811, #3484 ) ;
#6361 = ORIENTED_EDGE ( 'NONE', *, *, #3964, .T. ) ;
#6362 = ORIENTED_EDGE ( 'NONE', *, *, #3400, .F. ) ;
#6363 = CARTESIAN_POINT ( 'NONE',  ( 2.740000000000000213, 0.5149999999999976819, 0.6774776749089244099 ) ) ;
#6364 = PRODUCT_DEFINITION_SHAPE ( 'NONE', 'NONE',  #14350 ) ;
#6365 = CARTESIAN_POINT ( 'NONE',  ( 224.9999999999999716, -85.00000000000007105, 50.00000000000001421 ) ) ;
#6366 = PRODUCT_DEFINITION_CONTEXT ( 'detailed design', #3418, 'design' ) ;
#6367 = ORIENTED_EDGE ( 'NONE', *, *, #8242, .F. ) ;
#6368 = CARTESIAN_POINT ( 'NONE',  ( 79.99999999999971578, 35.00000000000000000, 10.00000000000000000 ) ) ;
#6369 = ADVANCED_FACE ( 'NONE', ( #1434 ), #1644, .T. ) ;
#6370 = DIRECTION ( 'NONE',  ( 1.000000000000000000, 0.000000000000000000, 0.000000000000000000 ) ) ;
#6371 = CARTESIAN_POINT ( 'NONE',  ( 4.197478902586992966, -0.8524102783748346290, -3.505063281295504041 ) ) ;
#6372 = PLANE ( 'NONE',  #1583 ) ;
#6373 =( LENGTH_UNIT ( ) NAMED_UNIT ( * ) SI_UNIT ( .MILLI., .METRE. ) );
#6374 = VECTOR ( 'NONE', #8040, 1000.000000000000000 ) ;
#6375 =( REPRESENTATION_RELATIONSHIP ('NONE','NONE', #11251, #9307 ) REPRESENTATION_RELATIONSHIP_WITH_TRANSFORMATION ( #7482 )SHAPE_REPRESENTATION_RELATIONSHIP( ) );
#6376 = AXIS2_PLACEMENT_3D ( 'NONE', #10264, #154, #292 ) ;
#6377 = CONTEXT_DEPENDENT_SHAPE_REPRESENTATION ( #9470, #1018 ) ;
#6378 = VERTEX_POINT ( 'NONE', #6083 ) ;
#6379 = ADVANCED_FACE ( 'NONE', ( #6010 ), #4721, .F. ) ;
#6380 = PLANE ( 'NONE',  #9614 ) ;
#6381 = ORIENTED_EDGE ( 'NONE', *, *, #10368, .F. ) ;
#6382 = DIRECTION ( 'NONE',  ( 1.000000000000000000, 0.000000000000000000, 0.000000000000000000 ) ) ;
#6383 = DIRECTION ( 'NONE',  ( -0.000000000000000000, 1.000000000000000000, -0.000000000000000000 ) ) ;
#6384 = EDGE_LOOP ( 'NONE', ( #9160, #14001 ) ) ;
#6385 = CARTESIAN_POINT ( 'NONE',  ( 347.0000000000000000, 8.660254037844390851, 200.0000000000000000 ) ) ;
#6386 = ORIENTED_EDGE ( 'NONE', *, *, #4985, .F. ) ;
#6387 = LINE ( 'NONE', #10888, #8711 ) ;
#6388 = CARTESIAN_POINT ( 'NONE',  ( 219.9999999999999716, -25.00000000000000000, -222.5000000000000853 ) ) ;
#6389 = VERTEX_POINT ( 'NONE', #10437 ) ;
#6390 = PRESENTATION_STYLE_ASSIGNMENT (( #10751 ) ) ;
#6391 = FACE_OUTER_BOUND ( 'NONE', #3361, .T. ) ;
#6392 = DIRECTION ( 'NONE',  ( 0.000000000000000000, 0.5000000000000009992, 0.8660254037844380415 ) ) ;
#6393 = ITEM_DEFINED_TRANSFORMATION ( 'NONE', 'NONE', #11406,  #14039 ) ;
#6394 = CARTESIAN_POINT ( 'NONE',  ( -4.211399284164270895, 2.459729995988205964, -3.751162237960538715 ) ) ;
#6395 = CIRCLE ( 'NONE', #7075, 4.250000000000000000 ) ;
#6396 = ORIENTED_EDGE ( 'NONE', *, *, #2963, .F. ) ;
#6397 = EDGE_LOOP ( 'NONE', ( #12782, #767, #10521, #13988 ) ) ;
#6398 = EDGE_CURVE ( 'NONE', #3114, #5927, #5868, .T. ) ;
#6399 = DIRECTION ( 'NONE',  ( 0.000000000000000000, 0.000000000000000000, 1.000000000000000000 ) ) ;
#6400 = ORIENTED_EDGE ( 'NONE', *, *, #6398, .F. ) ;
#6401 = DIRECTION ( 'NONE',  ( -1.000000000000000000, 0.000000000000000000, 0.000000000000000000 ) ) ;
#6402 = VERTEX_POINT ( 'NONE', #13539 ) ;
#6403 = VERTEX_POINT ( 'NONE', #4784 ) ;
#6404 = DIRECTION ( 'NONE',  ( 0.000000000000000000, 1.000000000000000000, 0.000000000000000000 ) ) ;
#6405 = ORIENTED_EDGE ( 'NONE', *, *, #7442, .T. ) ;
#6406 = DIRECTION ( 'NONE',  ( 1.000000000000000000, 0.000000000000000000, 0.000000000000000000 ) ) ;
#6407 = VECTOR ( 'NONE', #5929, 1000.000000000000000 ) ;
#6408 = CARTESIAN_POINT ( 'NONE',  ( -31.74999999999995737, 3.061616997868383634E-16, -2.500000000000000444 ) ) ;
#6409 = LINE ( 'NONE', #4163, #359 ) ;
#6410 = EDGE_CURVE ( 'NONE', #6238, #1677, #4932, .T. ) ;
#6411 = ADVANCED_FACE ( 'NONE', ( #1495 ), #1360, .F. ) ;
#6412 = VECTOR ( 'NONE', #11939, 1000.000000000000000 ) ;
#6413 = ADVANCED_FACE ( 'NONE', ( #12544 ), #8105, .F. ) ;
#6414 = CARTESIAN_POINT ( 'NONE',  ( 0.2500000000000002220, 4.898587196589412829E-16, -4.000000000000000000 ) ) ;
#6415 = CARTESIAN_POINT ( 'NONE',  ( 134.9999999999999432, -56.99999999999997158, -169.9999999999999716 ) ) ;
#6416 = ORIENTED_EDGE ( 'NONE', *, *, #12946, .T. ) ;
#6417 = CIRCLE ( 'NONE', #11051, 4.000000000000000000 ) ;
#6418 = ORIENTED_EDGE ( 'NONE', *, *, #14291, .F. ) ;
#6419 = AXIS2_PLACEMENT_3D ( 'NONE', #6515, #8543, #6444 ) ;
#6421 = CYLINDRICAL_SURFACE ( 'NONE', #8636, 5.000000000000004441 ) ;
#6420 = VECTOR ( 'NONE', #3797, 1000.000000000000000 ) ;
#6422 = VERTEX_POINT ( 'NONE', #8067 ) ;
#6423 = CARTESIAN_POINT ( 'NONE',  ( -30.00000000000002842, -25.00000000000000000, -250.0000000000000000 ) ) ;
#6424 = LINE ( 'NONE', #1102, #7459 ) ;
#6425 = CARTESIAN_POINT ( 'NONE',  ( 297.3499999999999659, -95.00000000000008527, 190.0000000000000000 ) ) ;
#6426 = VECTOR ( 'NONE', #9460, 1000.000000000000000 ) ;
#6427 = ORIENTED_EDGE ( 'NONE', *, *, #12971, .T. ) ;
#6428 = CIRCLE ( 'NONE', #3194, 2.500000000000002220 ) ;
#6429 = ADVANCED_FACE ( 'NONE', ( #11273 ), #4534, .F. ) ;
#6430 = DIRECTION ( 'NONE',  ( 0.000000000000000000, 1.000000000000000000, -1.287488025362403787E-15 ) ) ;
#6431 = VECTOR ( 'NONE', #8478, 1000.000000000000000 ) ;
#6432 = FACE_OUTER_BOUND ( 'NONE', #10071, .T. ) ;
#6433 = CIRCLE ( 'NONE', #5494, 0.2500000000000002220 ) ;
#6434 = DIRECTION ( 'NONE',  ( -1.000000000000000000, -0.000000000000000000, -0.000000000000000000 ) ) ;
#6435 = ORIENTED_EDGE ( 'NONE', *, *, #5164, .F. ) ;
#6436 = AXIS2_PLACEMENT_3D ( 'NONE', #1671, #5181, #5106 ) ;
#6437 = ORIENTED_EDGE ( 'NONE', *, *, #12821, .T. ) ;
#6438 = PLANE ( 'NONE',  #3703 ) ;
#6439 = CIRCLE ( 'NONE', #149, 10.00000000000000000 ) ;
#6440 = ADVANCED_FACE ( 'NONE', ( #1322 ), #71, .T. ) ;
#6441 = CARTESIAN_POINT ( 'NONE',  ( 201.0000000000000000, -85.00000000000007105, 180.0000000000000000 ) ) ;
#6442 = AXIS2_PLACEMENT_3D ( 'NONE', #5231, #6165, #3058 ) ;
#6443 = ORIENTED_EDGE ( 'NONE', *, *, #8961, .F. ) ;
#6444 = DIRECTION ( 'NONE',  ( -1.110223024625157487E-14, -1.000000000000000000, 0.000000000000000000 ) ) ;
#6445 = CARTESIAN_POINT ( 'NONE',  ( 305.4999999999999432, -95.00000000000008527, -190.0000000000000000 ) ) ;
#6446 = CARTESIAN_POINT ( 'NONE',  ( 0.000000000000000000, 0.000000000000000000, 0.000000000000000000 ) ) ;
#6447 =( LENGTH_UNIT ( ) NAMED_UNIT ( * ) SI_UNIT ( .MILLI., .METRE. ) );
#6448 = ITEM_DEFINED_TRANSFORMATION ( 'NONE', 'NONE', #9325,  #14039 ) ;
#6449 = CIRCLE ( 'NONE', #14087, 5.500000000000005329 ) ;
#6450 = EDGE_LOOP ( 'NONE', ( #8493, #9799 ) ) ;
#6451 = CARTESIAN_POINT ( 'NONE',  ( -30.00000000000002842, -225.0000000000000000, 169.9999999999999716 ) ) ;
#6452 = EDGE_LOOP ( 'NONE', ( #14041, #1223, #8945 ) ) ;
#6453 = EDGE_CURVE ( 'NONE', #566, #6215, #5032, .T. ) ;
#6454 = LINE ( 'NONE', #9581, #2365 ) ;
#6455 = LINE ( 'NONE', #9798, #7416 ) ;
#6456 = ADVANCED_BREP_SHAPE_REPRESENTATION ( '', ( #13134, #14039 ), #4225 ) ;
#6457 = ORIENTED_EDGE ( 'NONE', *, *, #6199, .F. ) ;
#6458 = EDGE_LOOP ( 'NONE', ( #1989, #10921, #12341, #12906 ) ) ;
#6459 = CARTESIAN_POINT ( 'NONE',  ( -304.9999999999999432, 45.00000000000001421, 40.00000000000000000 ) ) ;
#6460 = DIRECTION ( 'NONE',  ( 0.000000000000000000, 0.5000000000000011102, 0.8660254037844380415 ) ) ;
#6461 = EDGE_LOOP ( 'NONE', ( #8898, #7628, #7057, #8931 ) ) ;
#6462 = LINE ( 'NONE', #7404, #4584 ) ;
#6463 = ADVANCED_FACE ( 'NONE', ( #10320 ), #9098, .F. ) ;
#6464 = CARTESIAN_POINT ( 'NONE',  ( 197.5000000000000000, -80.00000000000007105, 55.00000000000001421 ) ) ;
#6465 = FACE_OUTER_BOUND ( 'NONE', #10281, .T. ) ;
#6466 = ITEM_DEFINED_TRANSFORMATION ( 'NONE', 'NONE', #9784,  #14039 ) ;
#6467 = DIRECTION ( 'NONE',  ( -1.000000000000000000, 0.000000000000000000, 0.000000000000000000 ) ) ;
#6468 = ORIENTED_EDGE ( 'NONE', *, *, #1262, .F. ) ;
#6469 = ORIENTED_EDGE ( 'NONE', *, *, #1797, .T. ) ;
#6470 = CARTESIAN_POINT ( 'NONE',  ( 8.000000000000000000, -4.837354856632045452E-15, 0.000000000000000000 ) ) ;
#6471 = VERTEX_POINT ( 'NONE', #13368 ) ;
#6472 = DIRECTION ( 'NONE',  ( 0.000000000000000000, -0.5000000000000011102, -0.8660254037844379305 ) ) ;
#6473 = CIRCLE ( 'NONE', #11804, 9.999999999999980460 ) ;
#6474 = VERTEX_POINT ( 'NONE', #12501 ) ;
#6475 = ORIENTED_EDGE ( 'NONE', *, *, #6343, .F. ) ;
#6476 = CARTESIAN_POINT ( 'NONE',  ( -144.9999999999999432, 55.00000000000001421, 40.00000000000000000 ) ) ;
#6477 = EDGE_LOOP ( 'NONE', ( #4100, #6350 ) ) ;
#6478 = AXIS2_PLACEMENT_3D ( 'NONE', #3713, #2411, #2697 ) ;
#6479 = CYLINDRICAL_SURFACE ( 'NONE', #10322, 2.649999999999985700 ) ;
#6480 = CARTESIAN_POINT ( 'NONE',  ( 1.799999999999996048, 1.236893267138826416E-15, 9.999999999999994671 ) ) ;
#6481 = CARTESIAN_POINT ( 'NONE',  ( -302.3499999999999659, 45.00000000000001421, 40.00000000000000000 ) ) ;
#6482 = EDGE_CURVE ( 'NONE', #7600, #5508, #4468, .T. ) ;
#6483 = DIRECTION ( 'NONE',  ( -0.000000000000000000, 0.000000000000000000, 1.000000000000000000 ) ) ;
#6484 = EDGE_CURVE ( 'NONE', #7334, #11965, #10347, .T. ) ;
#6485 = CARTESIAN_POINT ( 'NONE',  ( 305.0000000000000000, -36.99999999999997868, -180.0000000000000000 ) ) ;
#6486 = VECTOR ( 'NONE', #2577, 1000.000000000000000 ) ;
#6487 = DIRECTION ( 'NONE',  ( 0.000000000000000000, 0.000000000000000000, -1.000000000000000000 ) ) ;
#6488 = PRODUCT_DEFINITION_SHAPE ( 'NONE', 'NONE',  #14347 ) ;
#6489 = VERTEX_POINT ( 'NONE', #7780 ) ;
#6490 = ORIENTED_EDGE ( 'NONE', *, *, #977, .F. ) ;
#6491 = EDGE_CURVE ( 'NONE', #140, #1312, #4604, .T. ) ;
#6492 = CARTESIAN_POINT ( 'NONE',  ( 386.6666666666666288, -15.00000000000000000, 225.1500000000000625 ) ) ;
#6493 = ORIENTED_EDGE ( 'NONE', *, *, #2881, .T. ) ;
#6494 = DIRECTION ( 'NONE',  ( 0.8571673013836870192, 1.049727191973306873E-16, -0.5150380737757234151 ) ) ;
#6495 = PLANE ( 'NONE',  #4013 ) ;
#6496 = CARTESIAN_POINT ( 'NONE',  ( 3.678949249685231848, 0.000000000000000000, 0.000000000000000000 ) ) ;
#6497 = VERTEX_POINT ( 'NONE', #13510 ) ;
#6498 = VECTOR ( 'NONE', #3202, 1000.000000000000000 ) ;
#6499 = ADVANCED_FACE ( 'NONE', ( #2283 ), #12292, .F. ) ;
#6500 = CARTESIAN_POINT ( 'NONE',  ( 217.4999999999999147, -85.00000000000009948, 0.000000000000000000 ) ) ;
#6501 = AXIS2_PLACEMENT_3D ( 'NONE', #8322, #9493, #1793 ) ;
#6502 = CARTESIAN_POINT ( 'NONE',  ( -304.9999999999999432, -75.00000000000008527, 354.1421356237308942 ) ) ;
#6503 = DIRECTION ( 'NONE',  ( -1.000000000000000000, 0.000000000000000000, 0.000000000000000000 ) ) ;
#6504 = EDGE_LOOP ( 'NONE', ( #7133, #3450, #11412, #13954 ) ) ;
#6505 = VECTOR ( 'NONE', #7081, 1000.000000000000000 ) ;
#6506 =( REPRESENTATION_RELATIONSHIP ('NONE','NONE', #11251, #9778 ) REPRESENTATION_RELATIONSHIP_WITH_TRANSFORMATION ( #8620 )SHAPE_REPRESENTATION_RELATIONSHIP( ) );
#6507 = AXIS2_PLACEMENT_3D ( 'NONE', #7729, #5824, #3795 ) ;
#6508 = ORIENTED_EDGE ( 'NONE', *, *, #11183, .F. ) ;
#6509 = ADVANCED_FACE ( 'NONE', ( #13300, #5830, #6781 ), #217, .T. ) ;
#6510 = DIRECTION ( 'NONE',  ( -1.000000000000000000, -0.000000000000000000, -0.000000000000000000 ) ) ;
#6511 = EDGE_CURVE ( 'NONE', #5306, #7372, #8732, .T. ) ;
#6512 = AXIS2_PLACEMENT_3D ( 'NONE', #6414, #803, #12863 ) ;
#6513 = CARTESIAN_POINT ( 'NONE',  ( -4.211140560182196957, 2.431303136016537803, -3.745885042887433514 ) ) ;
#6514 = EDGE_LOOP ( 'NONE', ( #8787, #10386, #7314, #7127 ) ) ;
#6515 = CARTESIAN_POINT ( 'NONE',  ( 359.9999999999997726, 35.00000000000002842, 10.00000000000000000 ) ) ;
#6516 = ADVANCED_FACE ( 'NONE', ( #2498 ), #10048, .F. ) ;
#6517 = VECTOR ( 'NONE', #229, 1000.000000000000000 ) ;
#6518 = DIRECTION ( 'NONE',  ( 0.000000000000000000, 0.000000000000000000, -1.000000000000000000 ) ) ;
#6519 = CARTESIAN_POINT ( 'NONE',  ( 264.0000000000000000, 0.000000000000000000, -188.0000000000000000 ) ) ;
#6520 = CIRCLE ( 'NONE', #6512, 0.2500000000000002220 ) ;
#6521 = EDGE_LOOP ( 'NONE', ( #12767, #12332 ) ) ;
#6522 = LINE ( 'NONE', #8623, #2668 ) ;
#6523 = AXIS2_PLACEMENT_3D ( 'NONE', #3728, #1539, #288 ) ;
#6524 = ORIENTED_EDGE ( 'NONE', *, *, #2672, .T. ) ;
#6525 = CARTESIAN_POINT ( 'NONE',  ( 0.000000000000000000, -225.0000000000000000, 0.000000000000000000 ) ) ;
#6526 = CYLINDRICAL_SURFACE ( 'NONE', #6719, 5.500000000000005329 ) ;
#6527 = ORIENTED_EDGE ( 'NONE', *, *, #11731, .T. ) ;
#6528 = ORIENTED_EDGE ( 'NONE', *, *, #10557, .F. ) ;
#6529 = DIRECTION ( 'NONE',  ( 0.000000000000000000, 0.000000000000000000, -1.000000000000000000 ) ) ;
#6530 = UNCERTAINTY_MEASURE_WITH_UNIT (LENGTH_MEASURE( 1.000000000000000082E-05 ), #7539, 'distance_accuracy_value', 'NONE');
#6531 = CARTESIAN_POINT ( 'NONE',  ( 2.500000000000000000, 0.000000000000000000, 0.000000000000000000 ) ) ;
#6532 = ORIENTED_EDGE ( 'NONE', *, *, #12600, .T. ) ;
#6533 = CARTESIAN_POINT ( 'NONE',  ( 219.9999999999999716, -85.00000000000007105, 50.00000000000001421 ) ) ;
#6534 = DIRECTION ( 'NONE',  ( 0.000000000000000000, -0.000000000000000000, 1.000000000000000000 ) ) ;
#6535 = CARTESIAN_POINT ( 'NONE',  ( 1.794155980045909482, 0.000000000000000000, 0.000000000000000000 ) ) ;
#6536 = CARTESIAN_POINT ( 'NONE',  ( 299.9999999999999432, -75.00000000000008527, -190.0000000000000000 ) ) ;
#6537 = AXIS2_PLACEMENT_3D ( 'NONE', #3280, #9946, #12861 ) ;
#6538 = EDGE_CURVE ( 'NONE', #2405, #8981, #5755, .T. ) ;
#6539 = DIRECTION ( 'NONE',  ( -1.000000000000000000, 0.000000000000000000, 0.000000000000000000 ) ) ;
#6540 = CARTESIAN_POINT ( 'NONE',  ( 2.500000000000000000, 0.000000000000000000, 0.000000000000000000 ) ) ;
#6541 = AXIS2_PLACEMENT_3D ( 'NONE', #5745, #6832, #889 ) ;
#6542 = ORIENTED_EDGE ( 'NONE', *, *, #7204, .T. ) ;
#6543 = EDGE_LOOP ( 'NONE', ( #12547, #7520, #9847, #101 ) ) ;
#6544 = CYLINDRICAL_SURFACE ( 'NONE', #801, 2.649999999999985700 ) ;
#6545 = ORIENTED_EDGE ( 'NONE', *, *, #5577, .F. ) ;
#6546 = CARTESIAN_POINT ( 'NONE',  ( 0.000000000000000000, 0.000000000000000000, 0.000000000000000000 ) ) ;
#6547 = ORIENTED_EDGE ( 'NONE', *, *, #12747, .T. ) ;
#6548 = CIRCLE ( 'NONE', #8144, 2.649999999999985700 ) ;
#6549 = ORIENTED_EDGE ( 'NONE', *, *, #6048, .F. ) ;
#6550 = CARTESIAN_POINT ( 'NONE',  ( 137.3500000000000227, -75.00000000000008527, 169.9999999999999716 ) ) ;
#6551 = VERTEX_POINT ( 'NONE', #2422 ) ;
#6552 = DIRECTION ( 'NONE',  ( 0.000000000000000000, 0.000000000000000000, 1.000000000000000000 ) ) ;
#6553 = DIRECTION ( 'NONE',  ( 1.000000000000000000, 0.000000000000000000, 0.000000000000000000 ) ) ;
#6554 = CYLINDRICAL_SURFACE ( 'NONE', #14060, 2.649999999999985700 ) ;
#6555 =( GEOMETRIC_REPRESENTATION_CONTEXT ( 3 ) GLOBAL_UNCERTAINTY_ASSIGNED_CONTEXT ( ( #9589 ) ) GLOBAL_UNIT_ASSIGNED_CONTEXT ( ( #13225, #4524, #13356 ) ) REPRESENTATION_CONTEXT ( 'NONE', 'WORKASPACE' ) );
#6556 = CARTESIAN_POINT ( 'NONE',  ( 2.740000000000000213, 0.5150000000000035660, -0.9838866223905657904 ) ) ;
#6557 = DIRECTION ( 'NONE',  ( 0.000000000000000000, 0.000000000000000000, 1.000000000000000000 ) ) ;
#6558 = EDGE_CURVE ( 'NONE', #6497, #6109, #10257, .T. ) ;
#6559 = DIRECTION ( 'NONE',  ( 0.000000000000000000, 0.000000000000000000, -1.000000000000000000 ) ) ;
#6560 = CARTESIAN_POINT ( 'NONE',  ( 134.5000000000000000, -75.00000000000008527, 186.2999999999999829 ) ) ;
#6561 = VECTOR ( 'NONE', #666, 1000.000000000000000 ) ;
#6562 = ORIENTED_EDGE ( 'NONE', *, *, #8747, .T. ) ;
#6563 = ORIENTED_EDGE ( 'NONE', *, *, #1970, .T. ) ;
#6564 = AXIS2_PLACEMENT_3D ( 'NONE', #13446, #5124, #8366 ) ;
#6565 = EDGE_CURVE ( 'NONE', #7514, #3844, #13577, .T. ) ;
#6566 = CARTESIAN_POINT ( 'NONE',  ( 79.99999999999971578, 55.00000000000000711, 10.00000000000000000 ) ) ;
#6567 = ADVANCED_FACE ( 'NONE', ( #1464 ), #2862, .F. ) ;
#6568 = VERTEX_POINT ( 'NONE', #1534 ) ;
#6569 = DIRECTION ( 'NONE',  ( 1.000000000000000000, 0.000000000000000000, 0.000000000000000000 ) ) ;
#6570 = DIRECTION ( 'NONE',  ( -1.000000000000000000, -0.000000000000000000, -0.000000000000000000 ) ) ;
#6571 = CARTESIAN_POINT ( 'NONE',  ( 2.740000000000000213, -0.5150000000000034550, 0.9838866223909985553 ) ) ;
#6572 = APPLICATION_CONTEXT ( 'automotive_design' ) ;
#6573 = ORIENTED_EDGE ( 'NONE', *, *, #1512, .F. ) ;
#6574 = CARTESIAN_POINT ( 'NONE',  ( 53.33333333333330017, -20.00000000000000000, 222.5000000000000853 ) ) ;
#6575 = LINE ( 'NONE', #4478, #10887 ) ;
#6576 = PRODUCT_DEFINITION_SHAPE ( 'NONE', 'NONE',  #13043 ) ;
#6577 = CARTESIAN_POINT ( 'NONE',  ( 0.000000000000000000, 0.000000000000000000, 186.0000000000000000 ) ) ;
#6578 = ORIENTED_EDGE ( 'NONE', *, *, #2005, .F. ) ;
#6579 = EDGE_CURVE ( 'NONE', #9829, #10653, #425, .T. ) ;
#6580 = CARTESIAN_POINT ( 'NONE',  ( 1.800000000000002931, 0.000000000000000000, 0.000000000000000000 ) ) ;
#6581 = EDGE_CURVE ( 'NONE', #3798, #4511, #5276, .T. ) ;
#6582 = DIRECTION ( 'NONE',  ( -0.000000000000000000, 0.8660254037844392627, 0.4999999999999990008 ) ) ;
#6583 = ORIENTED_EDGE ( 'NONE', *, *, #11718, .T. ) ;
#6584 = DIRECTION ( 'NONE',  ( -1.000000000000000000, 0.000000000000000000, 0.000000000000000000 ) ) ;
#6585 = FACE_OUTER_BOUND ( 'NONE', #10430, .T. ) ;
#6586 = ADVANCED_FACE ( 'NONE', ( #11632 ), #5118, .F. ) ;
#6587 = EDGE_CURVE ( 'NONE', #7398, #12108, #3799, .T. ) ;
#6588 = CARTESIAN_POINT ( 'NONE',  ( -304.9999999999999432, -75.00000000000008527, 354.1421356237308942 ) ) ;
#6589 = DIRECTION ( 'NONE',  ( 1.000000000000000000, 6.123233995736766036E-17, -6.123233995736764803E-17 ) ) ;
#6590 = EDGE_CURVE ( 'NONE', #2418, #915, #6118, .T. ) ;
#6591 = CONTEXT_DEPENDENT_SHAPE_REPRESENTATION ( #821, #14234 ) ;
#6592 = ORIENTED_EDGE ( 'NONE', *, *, #11811, .F. ) ;
#6593 = PLANE ( 'NONE',  #13550 ) ;
#6594 = ORIENTED_EDGE ( 'NONE', *, *, #8371, .T. ) ;
#6595 = CARTESIAN_POINT ( 'NONE',  ( 0.000000000000000000, 0.000000000000000000, 0.000000000000000000 ) ) ;
#6596 = DIRECTION ( 'NONE',  ( 1.000000000000000000, 0.000000000000000000, -0.000000000000000000 ) ) ;
#6597 = VERTEX_POINT ( 'NONE', #11703 ) ;
#6598 = VERTEX_POINT ( 'NONE', #13730 ) ;
#6599 = CARTESIAN_POINT ( 'NONE',  ( -5.000000000000000888, 8.660254037844390851, 210.0000000000000000 ) ) ;
#6600 = CARTESIAN_POINT ( 'NONE',  ( 2.500000000000000000, 2.357898499370433054, -1.951563910473907981E-15 ) ) ;
#6601 = VECTOR ( 'NONE', #3938, 1000.000000000000000 ) ;
#6602 = DIRECTION ( 'NONE',  ( 0.000000000000000000, 0.000000000000000000, -1.000000000000000000 ) ) ;
#6603 = CARTESIAN_POINT ( 'NONE',  ( 145.5000000000000284, -95.00000000000008527, 190.0000000000000000 ) ) ;
#6604 = DIRECTION ( 'NONE',  ( 1.000000000000000000, 0.000000000000000000, 0.000000000000000000 ) ) ;
#6605 = SHAPE_REPRESENTATION_RELATIONSHIP ( 'NONE' , 'NONE' ,  #9778, #9567 ) ;
#6606 = CARTESIAN_POINT ( 'NONE',  ( 2.500000000000000000, 2.357898499370433054, -1.951563910473907981E-15 ) ) ;
#6607 = CARTESIAN_POINT ( 'NONE',  ( -4.197477534772231955, 0.8522413273724368521, -3.505042416683225692 ) ) ;
#6608 = ORIENTED_EDGE ( 'NONE', *, *, #5273, .F. ) ;
#6609 = ORIENTED_EDGE ( 'NONE', *, *, #7469, .F. ) ;
#6610 = DIRECTION ( 'NONE',  ( -0.000000000000000000, 1.000000000000000000, -0.000000000000000000 ) ) ;
#6611 = AXIS2_PLACEMENT_3D ( 'NONE', #1225, #5660, #10156 ) ;
#6612 = EDGE_LOOP ( 'NONE', ( #1194, #1508, #11295, #6963 ) ) ;
#6613 = DIRECTION ( 'NONE',  ( -1.000000000000000000, 0.000000000000000000, -0.000000000000000000 ) ) ;
#6614 = EDGE_CURVE ( 'NONE', #14219, #3774, #10544, .T. ) ;
#6615 = EDGE_LOOP ( 'NONE', ( #4771, #6998, #8572, #9527 ) ) ;
#6616 = LINE ( 'NONE', #12065, #5493 ) ;
#6617 = ORIENTED_EDGE ( 'NONE', *, *, #10733, .T. ) ;
#6618 = DIRECTION ( 'NONE',  ( -0.000000000000000000, -0.000000000000000000, -1.000000000000000000 ) ) ;
#6619 = CARTESIAN_POINT ( 'NONE',  ( 140.0000000000000000, -95.00000000000008527, -190.0000000000000000 ) ) ;
#6620 = PLANE ( 'NONE',  #5489 ) ;
#6621 = CARTESIAN_POINT ( 'NONE',  ( 20.55500000000001748, 3.061616997868384127E-16, -2.500000000000000888 ) ) ;
#6622 = AXIS2_PLACEMENT_3D ( 'NONE', #6694, #13288, #8938 ) ;
#6623 = FILL_AREA_STYLE ('',( #7975 ) ) ;
#6624 = CIRCLE ( 'NONE', #14023, 9.999999999999994671 ) ;
#6625 = CARTESIAN_POINT ( 'NONE',  ( 53.33333333333330017, -25.00000000000000000, -225.1500000000000625 ) ) ;
#6626 = CYLINDRICAL_SURFACE ( 'NONE', #12443, 2.649999999999985700 ) ;
#6627 = ORIENTED_EDGE ( 'NONE', *, *, #2479, .T. ) ;
#6628 = ORIENTED_EDGE ( 'NONE', *, *, #6989, .F. ) ;
#6629 = CARTESIAN_POINT ( 'NONE',  ( 4.999999999999999112, 8.660254037844390851, 200.0000000000000000 ) ) ;
#6630 = VECTOR ( 'NONE', #14206, 1000.000000000000000 ) ;
#6631 = EDGE_LOOP ( 'NONE', ( #445, #4742 ) ) ;
#6632 = CARTESIAN_POINT ( 'NONE',  ( -1.999999999999998224, 0.000000000000000000, 0.000000000000000000 ) ) ;
#6633 = FACE_OUTER_BOUND ( 'NONE', #10319, .T. ) ;
#6634 = VECTOR ( 'NONE', #4285, 1000.000000000000000 ) ;
#6635 =( LENGTH_UNIT ( ) NAMED_UNIT ( * ) SI_UNIT ( .MILLI., .METRE. ) );
#6636 = VERTEX_POINT ( 'NONE', #5041 ) ;
#6637 = AXIS2_PLACEMENT_3D ( 'NONE', #7756, #8646, #7617 ) ;
#6638 = DIRECTION ( 'NONE',  ( -1.000000000000000000, -0.000000000000000000, -0.000000000000000000 ) ) ;
#6639 = CARTESIAN_POINT ( 'NONE',  ( 0.000000000000000000, 0.000000000000000000, 190.0000000000000000 ) ) ;
#6640 = EDGE_CURVE ( 'NONE', #611, #6568, #1606, .T. ) ;
#6641 = CONICAL_SURFACE ( 'NONE', #11772, 2.500000000000002220, 1.029744260000002631 ) ;
#6642 = AXIS2_PLACEMENT_3D ( 'NONE', #9634, #13977, #2892 ) ;
#6643 = DIRECTION ( 'NONE',  ( 0.4461977533473793778, 0.8949343913984707521, -1.884057886186824742E-16 ) ) ;
#6644 = FACE_OUTER_BOUND ( 'NONE', #11694, .T. ) ;
#6645 = CIRCLE ( 'NONE', #10579, 13.29999999999999893 ) ;
#6646 = ORIENTED_EDGE ( 'NONE', *, *, #8884, .F. ) ;
#6647 = LINE ( 'NONE', #1036, #9275 ) ;
#6648 = AXIS2_PLACEMENT_3D ( 'NONE', #1569, #9422, #2609 ) ;
#6649 = CARTESIAN_POINT ( 'NONE',  ( 236.4999999999999432, -85.00000000000007105, 55.00000000000001421 ) ) ;
#6650 = CIRCLE ( 'NONE', #5048, 13.50000000000000000 ) ;
#6651 = FACE_BOUND ( 'NONE', #4748, .T. ) ;
#6652 = ORIENTED_EDGE ( 'NONE', *, *, #9512, .F. ) ;
#6653 = CARTESIAN_POINT ( 'NONE',  ( 2.000000000000001776, 0.000000000000000000, 0.000000000000000000 ) ) ;
#6654 = AXIS2_PLACEMENT_3D ( 'NONE', #7492, #8502, #2785 ) ;
#6655 = AXIS2_PLACEMENT_3D ( 'NONE', #4216, #4142, #8635 ) ;
#6656 = DIRECTION ( 'NONE',  ( 0.000000000000000000, 0.000000000000000000, 1.000000000000000000 ) ) ;
#6657 = EDGE_CURVE ( 'NONE', #12287, #9466, #2713, .T. ) ;
#6658 = FACE_BOUND ( 'NONE', #13900, .T. ) ;
#6659 = DIRECTION ( 'NONE',  ( 0.000000000000000000, 0.000000000000000000, 1.000000000000000000 ) ) ;
#6660 = VECTOR ( 'NONE', #10990, 1000.000000000000000 ) ;
#6661 = ORIENTED_EDGE ( 'NONE', *, *, #5851, .F. ) ;
#6662 = CIRCLE ( 'NONE', #12450, 2.649999999999985700 ) ;
#6663 = CARTESIAN_POINT ( 'NONE',  ( 4.999999999999999112, 8.660254037844390851, 200.0000000000000000 ) ) ;
#6664 = TOROIDAL_SURFACE ( 'NONE', #9649, 11.75000000000000000, 1.050000000000000266 ) ;
#6665 = VERTEX_POINT ( 'NONE', #8208 ) ;
#6666 = DIRECTION ( 'NONE',  ( -0.000000000000000000, -0.000000000000000000, 1.000000000000000000 ) ) ;
#6667 = EDGE_CURVE ( 'NONE', #7915, #5881, #12638, .T. ) ;
#6668 = EDGE_CURVE ( 'NONE', #4723, #5974, #10122, .T. ) ;
#6669 = ORIENTED_EDGE ( 'NONE', *, *, #14180, .F. ) ;
#6670 = ORIENTED_EDGE ( 'NONE', *, *, #1080, .T. ) ;
#6671 = DIRECTION ( 'NONE',  ( 0.000000000000000000, 0.000000000000000000, -1.000000000000000000 ) ) ;
#6672 = VECTOR ( 'NONE', #6861, 1000.000000000000000 ) ;
#6673 = CARTESIAN_POINT ( 'NONE',  ( 136.6666666666666288, -20.00000000000000000, 222.5000000000000853 ) ) ;
#6674 = DIRECTION ( 'NONE',  ( 0.000000000000000000, 0.000000000000000000, 1.000000000000000000 ) ) ;
#6675 = EDGE_CURVE ( 'NONE', #4963, #5710, #12856, .T. ) ;
#6676 = CIRCLE ( 'NONE', #152, 2.041999999999999815 ) ;
#6677 = CARTESIAN_POINT ( 'NONE',  ( 302.6499999999999204, -95.00000000000008527, 186.2999999999999829 ) ) ;
#6678 = CARTESIAN_POINT ( 'NONE',  ( -20.63749999999999929, 0.000000000000000000, 0.000000000000000000 ) ) ;
#6679 = CARTESIAN_POINT ( 'NONE',  ( 319.9999999999999432, -225.0010000000000048, -19.99999999999998934 ) ) ;
#6680 =( NAMED_UNIT ( * ) PLANE_ANGLE_UNIT ( ) SI_UNIT ( $, .RADIAN. ) );
#6681 = CYLINDRICAL_SURFACE ( 'NONE', #876, 2.649999999999985700 ) ;
#6682 = DIRECTION ( 'NONE',  ( -0.000000000000000000, 0.000000000000000000, 1.000000000000000000 ) ) ;
#6683 = ORIENTED_EDGE ( 'NONE', *, *, #4535, .T. ) ;
#6684 = EDGE_LOOP ( 'NONE', ( #1287, #1224 ) ) ;
#6685 = CARTESIAN_POINT ( 'NONE',  ( 217.4999999999999147, -85.00000000000009948, -17.55500000000000327 ) ) ;
#6686 = ORIENTED_EDGE ( 'NONE', *, *, #13377, .T. ) ;
#6687 = FACE_BOUND ( 'NONE', #12851, .T. ) ;
#6688 = EDGE_CURVE ( 'NONE', #13943, #7291, #12793, .T. ) ;
#6689 = AXIS2_PLACEMENT_3D ( 'NONE', #1756, #6348, #11860 ) ;
#6690 = ORIENTED_EDGE ( 'NONE', *, *, #3498, .F. ) ;
#6691 = ADVANCED_FACE ( 'NONE', ( #4966, #12715, #2930, #7343, #11779, #353, #3724, #4824 ), #2787, .T. ) ;
#6692 = CARTESIAN_POINT ( 'NONE',  ( -25.39999999999996305, 0.000000000000000000, 4.749999999999999112 ) ) ;
#6693 = EDGE_LOOP ( 'NONE', ( #7933, #737, #4941, #14118 ) ) ;
#6694 = CARTESIAN_POINT ( 'NONE',  ( 386.6666666666666288, -14.99999999999999822, 222.5000000000000853 ) ) ;
#6695 = PRODUCT_DEFINITION_SHAPE ( 'NONE', 'NONE',  #14329 ) ;
#6696 = DIRECTION ( 'NONE',  ( 1.000000000000000000, 0.000000000000000000, 0.000000000000000000 ) ) ;
#6697 = CARTESIAN_POINT ( 'NONE',  ( 0.2277608394786177770, 0.000000000000000000, 0.000000000000000000 ) ) ;
#6698 = EDGE_CURVE ( 'NONE', #10653, #7761, #12576, .T. ) ;
#6699 = FACE_OUTER_BOUND ( 'NONE', #11664, .T. ) ;
#6700 =( NAMED_UNIT ( * ) SI_UNIT ( $, .STERADIAN. ) SOLID_ANGLE_UNIT ( ) );
#6701 = DIRECTION ( 'NONE',  ( -0.000000000000000000, -0.000000000000000000, 1.000000000000000000 ) ) ;
#6702 = ORIENTED_EDGE ( 'NONE', *, *, #8177, .T. ) ;
#6703 = AXIS2_PLACEMENT_3D ( 'NONE', #9357, #2538, #393 ) ;
#6704 = ORIENTED_EDGE ( 'NONE', *, *, #8018, .F. ) ;
#6705 = CARTESIAN_POINT ( 'NONE',  ( 3.900000000000000799, 0.000000000000000000, 0.000000000000000000 ) ) ;
#6706 = ORIENTED_EDGE ( 'NONE', *, *, #12747, .F. ) ;
#6707 = CARTESIAN_POINT ( 'NONE',  ( 299.9999999999999432, -75.00000000000008527, -169.9999999999999716 ) ) ;
#6708 = DIRECTION ( 'NONE',  ( -1.000000000000000000, 0.000000000000000000, -0.000000000000000000 ) ) ;
#6709 = EDGE_LOOP ( 'NONE', ( #8146, #10815, #3057, #13297 ) ) ;
#6710 = CIRCLE ( 'NONE', #3472, 0.8509999999999999787 ) ;
#6711 = LINE ( 'NONE', #9837, #7891 ) ;
#6712 = DIRECTION ( 'NONE',  ( -0.000000000000000000, -0.000000000000000000, -1.000000000000000000 ) ) ;
#6713 = CARTESIAN_POINT ( 'NONE',  ( -145.0000000000000284, -95.00000000000008527, 30.00000000000000000 ) ) ;
#6714 = DIRECTION ( 'NONE',  ( 1.000000000000000000, 0.000000000000000000, -0.000000000000000000 ) ) ;
#6715 = EDGE_CURVE ( 'NONE', #9739, #2036, #11485, .T. ) ;
#6716 = VERTEX_POINT ( 'NONE', #13075 ) ;
#6717 = VECTOR ( 'NONE', #5480, 1000.000000000000000 ) ;
#6718 = DIRECTION ( 'NONE',  ( 1.000000000000000000, 0.000000000000000000, 0.000000000000000000 ) ) ;
#6719 = AXIS2_PLACEMENT_3D ( 'NONE', #5435, #11023, #9859 ) ;
#6720 = DIRECTION ( 'NONE',  ( -0.000000000000000000, 1.000000000000000000, -0.000000000000000000 ) ) ;
#6721 = LINE ( 'NONE', #22, #3652 ) ;
#6722 =( GEOMETRIC_REPRESENTATION_CONTEXT ( 3 ) GLOBAL_UNCERTAINTY_ASSIGNED_CONTEXT ( ( #5194 ) ) GLOBAL_UNIT_ASSIGNED_CONTEXT ( ( #5818, #2557, #11838 ) ) REPRESENTATION_CONTEXT ( 'NONE', 'WORKASPACE' ) );
#6723 = VERTEX_POINT ( 'NONE', #8798 ) ;
#6724 = DIRECTION ( 'NONE',  ( 0.5000000000000013323, -0.8660254037844379305, 0.000000000000000000 ) ) ;
#6725 = B_SPLINE_CURVE_WITH_KNOTS ( 'NONE', 3,
 ( #10573, #11733, #3821, #1560, #12532, #1635, #2596, #12820 ),
 .UNSPECIFIED., .F., .F.,
 ( 4, 2, 2, 4 ),
 ( 2.465131517390770070E-07, 0.001183067374689869946, 0.001774477805458935659, 0.002365888236228001588 ),
 .UNSPECIFIED. ) ;
#6726 = CARTESIAN_POINT ( 'NONE',  ( 2.499999999999999556, 0.000000000000000000, 3.469446951953614189E-15 ) ) ;
#6727 = LINE ( 'NONE', #3191, #12492 ) ;
#6728 = DIRECTION ( 'NONE',  ( -1.000000000000000000, 0.000000000000000000, 0.000000000000000000 ) ) ;
#6729 = AXIS2_PLACEMENT_3D ( 'NONE', #10069, #6666, #8915 ) ;
#6730 = VECTOR ( 'NONE', #10150, 1000.000000000000000 ) ;
#6731 = EDGE_LOOP ( 'NONE', ( #6592, #10353 ) ) ;
#6732 = CARTESIAN_POINT ( 'NONE',  ( 1.567478505476134606E-15, 4.618802153517012066, -3.433295621305382905 ) ) ;
#6733 = ORIENTED_EDGE ( 'NONE', *, *, #11986, .F. ) ;
#6734 = LINE ( 'NONE', #1208, #440 ) ;
#6735 = EDGE_CURVE ( 'NONE', #3667, #9074, #5009, .T. ) ;
#6736 = EDGE_CURVE ( 'NONE', #10043, #7698, #6854, .T. ) ;
#6737 = CONICAL_SURFACE ( 'NONE', #453, 2.500000000000002220, 1.029744260000002631 ) ;
#6738 = ORIENTED_EDGE ( 'NONE', *, *, #7024, .T. ) ;
#6739 = ORIENTED_EDGE ( 'NONE', *, *, #6581, .F. ) ;
#6740 = CARTESIAN_POINT ( 'NONE',  ( -302.4999999999999432, -75.00000000000008527, 339.9999999999999432 ) ) ;
#6741 = CARTESIAN_POINT ( 'NONE',  ( -3.453038570459499024, -2.625189405340453419, -3.535263753545272891 ) ) ;
#6742 = CARTESIAN_POINT ( 'NONE',  ( 219.9999999999999716, -85.00000000000007105, 169.9999999999999716 ) ) ;
#6743 = FACE_BOUND ( 'NONE', #190, .T. ) ;
#6744 = CARTESIAN_POINT ( 'NONE',  ( -1.999999999999998224, 0.000000000000000000, 0.000000000000000000 ) ) ;
#6745 = DIRECTION ( 'NONE',  ( -1.000000000000000000, 0.000000000000000000, 0.000000000000000000 ) ) ;
#6746 = DIRECTION ( 'NONE',  ( -0.000000000000000000, -0.000000000000000000, -1.000000000000000000 ) ) ;
#6747 = CONTEXT_DEPENDENT_SHAPE_REPRESENTATION ( #6962, #13080 ) ;
#6748 = CARTESIAN_POINT ( 'NONE',  ( 53.33333333333330017, -20.00000000000000000, 222.5000000000000853 ) ) ;
#6749 = ORIENTED_EDGE ( 'NONE', *, *, #2424, .F. ) ;
#6750 = EDGE_LOOP ( 'NONE', ( #11100, #13181, #13851, #6805 ) ) ;
#6751 = CARTESIAN_POINT ( 'NONE',  ( 140.0000000000000000, -95.00000000000008527, 190.0000000000000000 ) ) ;
#6752 = EDGE_LOOP ( 'NONE', ( #1276, #652, #9543, #7396 ) ) ;
#6753 = LINE ( 'NONE', #1366, #3089 ) ;
#6754 = ADVANCED_FACE ( 'NONE', ( #3228, #8581 ), #11929, .F. ) ;
#6755 = EDGE_CURVE ( 'NONE', #981, #13072, #5462, .T. ) ;
#6756 = VERTEX_POINT ( 'NONE', #9677 ) ;
#6757 = DIRECTION ( 'NONE',  ( 0.000000000000000000, 0.000000000000000000, -1.000000000000000000 ) ) ;
#6758 = ORIENTED_EDGE ( 'NONE', *, *, #434, .T. ) ;
#6759 = DIRECTION ( 'NONE',  ( 0.000000000000000000, 0.000000000000000000, 1.000000000000000000 ) ) ;
#6760 = CARTESIAN_POINT ( 'NONE',  ( 0.000000000000000000, 0.000000000000000000, -190.0000000000000000 ) ) ;
#6761 = VECTOR ( 'NONE', #2868, 1000.000000000000000 ) ;
#6762 = DIRECTION ( 'NONE',  ( 0.000000000000000000, -0.000000000000000000, 1.000000000000000000 ) ) ;
#6763 = AXIS2_PLACEMENT_3D ( 'NONE', #14062, #8553, #10883 ) ;
#6764 = DIRECTION ( 'NONE',  ( 0.000000000000000000, 0.000000000000000000, -1.000000000000000000 ) ) ;
#6765 = STYLED_ITEM ( 'NONE', ( #8466 ), #5928 ) ;
#6766 = DIRECTION ( 'NONE',  ( 6.123233995736766036E-17, 0.000000000000000000, -1.000000000000000000 ) ) ;
#6767 = EDGE_CURVE ( 'NONE', #13397, #10177, #5254, .T. ) ;
#6768 = EDGE_CURVE ( 'NONE', #8550, #10315, #868, .T. ) ;
#6769 = LINE ( 'NONE', #2559, #366 ) ;
#6770 = ORIENTED_EDGE ( 'NONE', *, *, #12428, .T. ) ;
#6771 = EDGE_CURVE ( 'NONE', #9211, #6099, #1219, .T. ) ;
#6772 = VERTEX_POINT ( 'NONE', #934 ) ;
#6773 = AXIS2_PLACEMENT_3D ( 'NONE', #9355, #3909, #2608 ) ;
#6774 = EDGE_LOOP ( 'NONE', ( #6562, #7917, #13841, #13032 ) ) ;
#6775 = EDGE_CURVE ( 'NONE', #5337, #9602, #13547, .T. ) ;
#6776 = CARTESIAN_POINT ( 'NONE',  ( 228.6602540378443393, -90.00000000000007105, 170.0000000000000000 ) ) ;
#6777 = AXIS2_PLACEMENT_3D ( 'NONE', #3538, #7942, #2441 ) ;
#6778 = ORIENTED_EDGE ( 'NONE', *, *, #7739, .T. ) ;
#6779 = CARTESIAN_POINT ( 'NONE',  ( -2.682243648011671588, -3.070208061305317759, -0.04852650426602272971 ) ) ;
#6780 = VECTOR ( 'NONE', #12337, 1000.000000000000000 ) ;
#6781 = FACE_OUTER_BOUND ( 'NONE', #10534, .T. ) ;
#6782 = FACE_OUTER_BOUND ( 'NONE', #12692, .T. ) ;
#6783 =( REPRESENTATION_RELATIONSHIP ('NONE','NONE', #11251, #9307 ) REPRESENTATION_RELATIONSHIP_WITH_TRANSFORMATION ( #9358 )SHAPE_REPRESENTATION_RELATIONSHIP( ) );
#6785 = CIRCLE ( 'NONE', #4246, 4.250000000000000000 ) ;
#6784 = AXIS2_PLACEMENT_3D ( 'NONE', #10857, #13166, #5272 ) ;
#6786 = DIRECTION ( 'NONE',  ( 0.000000000000000000, 0.4999999999999993339, -0.8660254037844390407 ) ) ;
#6787 = CARTESIAN_POINT ( 'NONE',  ( 4.203935335434060505, 1.640780671294165272, -3.598452447879202598 ) ) ;
#6788 = ORIENTED_EDGE ( 'NONE', *, *, #6289, .F. ) ;
#6789 = DIRECTION ( 'NONE',  ( -0.000000000000000000, -1.000000000000000000, -0.000000000000000000 ) ) ;
#6790 = MECHANICAL_DESIGN_GEOMETRIC_PRESENTATION_REPRESENTATION (  '', ( #4908 ), #7931 ) ;
#6791 = DIRECTION ( 'NONE',  ( 1.000000000000000000, 0.000000000000000000, 0.000000000000000000 ) ) ;
#6792 = ORIENTED_EDGE ( 'NONE', *, *, #7135, .T. ) ;
#6793 = VECTOR ( 'NONE', #1725, 1000.000000000000000 ) ;
#6794 = CARTESIAN_POINT ( 'NONE',  ( 307.5000000000000000, -56.99999999999997158, -180.0000000000000000 ) ) ;
#6795 = LINE ( 'NONE', #2435, #1661 ) ;
#6796 = FACE_OUTER_BOUND ( 'NONE', #6693, .T. ) ;
#6797 = EDGE_CURVE ( 'NONE', #3720, #3167, #4074, .T. ) ;
#6798 = EDGE_LOOP ( 'NONE', ( #14133, #3611, #6259, #8385 ) ) ;
#6799 = CARTESIAN_POINT ( 'NONE',  ( -299.9999999999999432, -95.00000000000008527, 30.00000000000002842 ) ) ;
#6800 = FACE_OUTER_BOUND ( 'NONE', #11265, .T. ) ;
#6801 = DIRECTION ( 'NONE',  ( 0.000000000000000000, 0.000000000000000000, 1.000000000000000000 ) ) ;
#6802 = ORIENTED_EDGE ( 'NONE', *, *, #6214, .F. ) ;
#6803 = CARTESIAN_POINT ( 'NONE',  ( 136.6666666666666288, -20.00000000000000000, 225.1500000000000625 ) ) ;
#6804 = PRODUCT_DEFINITION_SHAPE ( 'NONE', 'NONE',  #2142 ) ;
#6805 = ORIENTED_EDGE ( 'NONE', *, *, #12577, .F. ) ;
#6806 = CARTESIAN_POINT ( 'NONE',  ( -4.000000000000000000, -1.560351142792950618, -0.2242961665059814425 ) ) ;
#6807 = ORIENTED_EDGE ( 'NONE', *, *, #3485, .F. ) ;
#6808 = ORIENTED_EDGE ( 'NONE', *, *, #9552, .F. ) ;
#6809 = FACE_OUTER_BOUND ( 'NONE', #6615, .T. ) ;
#6810 = CARTESIAN_POINT ( 'NONE',  ( 0.1756481739660539498, -4.720212674038995360, -3.469390959564070620 ) ) ;
#6811 = CARTESIAN_POINT ( 'NONE',  ( 305.0000000000000000, -36.99999999999997868, -180.0000000000000000 ) ) ;
#6812 = CARTESIAN_POINT ( 'NONE',  ( 136.6666666666666288, -15.00000000000000000, 222.5000000000000853 ) ) ;
#6813 = CARTESIAN_POINT ( 'NONE',  ( -3.333333333333332149, -2.694301256218264218, -3.300726591567082036 ) ) ;
#6814 = DIRECTION ( 'NONE',  ( -0.000000000000000000, -0.000000000000000000, -1.000000000000000000 ) ) ;
#6815 = CARTESIAN_POINT ( 'NONE',  ( 4.204015924366189871, -1.626724848190933548, -3.610627190413393084 ) ) ;
#6816 = EDGE_CURVE ( 'NONE', #7102, #1514, #11995, .T. ) ;
#6817 = ORIENTED_EDGE ( 'NONE', *, *, #6938, .F. ) ;
#6818 = ORIENTED_EDGE ( 'NONE', *, *, #4805, .F. ) ;
#6819 = DIRECTION ( 'NONE',  ( 0.000000000000000000, 0.000000000000000000, 1.000000000000000000 ) ) ;
#6820 = VERTEX_POINT ( 'NONE', #4381 ) ;
#6821 = DIRECTION ( 'NONE',  ( -0.000000000000000000, -0.000000000000000000, -1.000000000000000000 ) ) ;
#6822 = AXIS2_PLACEMENT_3D ( 'NONE', #14002, #7266, #7125 ) ;
#6823 = VERTEX_POINT ( 'NONE', #13221 ) ;
#6824 = LINE ( 'NONE', #6021, #1786 ) ;
#6825 = VERTEX_POINT ( 'NONE', #2123 ) ;
#6826 = CARTESIAN_POINT ( 'NONE',  ( 0.000000000000000000, 0.000000000000000000, 3.469446951953614189E-15 ) ) ;
#6827 = DIRECTION ( 'NONE',  ( 1.000000000000000000, 0.000000000000000000, -0.000000000000000000 ) ) ;
#6828 = LINE ( 'NONE', #1735, #4335 ) ;
#6829 = CARTESIAN_POINT ( 'NONE',  ( -6.259644161404859044E-16, -4.618802153517026277, -3.504271511727133248 ) ) ;
#6830 =( LENGTH_UNIT ( ) NAMED_UNIT ( * ) SI_UNIT ( .MILLI., .METRE. ) );
#6831 = ADVANCED_FACE ( 'NONE', ( #2193 ), #6479, .F. ) ;
#6832 = DIRECTION ( 'NONE',  ( -1.000000000000000000, 0.000000000000000000, 6.123233995736766036E-17 ) ) ;
#6833 = PRODUCT_DEFINITION ( 'UNKNOWN', '', #4477, #4127 ) ;
#6834 = FACE_OUTER_BOUND ( 'NONE', #6129, .T. ) ;
#6835 = ORIENTED_EDGE ( 'NONE', *, *, #2566, .T. ) ;
#6836 = AXIS2_PLACEMENT_3D ( 'NONE', #1330, #3460, #2364 ) ;
#6837 = ORIENTED_EDGE ( 'NONE', *, *, #11911, .F. ) ;
#6838 = ORIENTED_EDGE ( 'NONE', *, *, #9285, .F. ) ;
#6839 = CARTESIAN_POINT ( 'NONE',  ( -3.974357786152442180E-13, 4.796734841935204052, -3.721909803043259579 ) ) ;
#6840 = ORIENTED_EDGE ( 'NONE', *, *, #8961, .T. ) ;
#6841 = DIRECTION ( 'NONE',  ( -0.000000000000000000, -0.000000000000000000, -1.000000000000000000 ) ) ;
#6842 = CARTESIAN_POINT ( 'NONE',  ( 434.9999999999999432, -8.660254037844389075, 199.9990000000000236 ) ) ;
#6843 = EDGE_CURVE ( 'NONE', #8753, #11376, #7305, .T. ) ;
#6844 = ADVANCED_FACE ( 'NONE', ( #14092 ), #3008, .F. ) ;
#6845 = AXIS2_PLACEMENT_3D ( 'NONE', #5193, #9822, #6406 ) ;
#6846 = CARTESIAN_POINT ( 'NONE',  ( 219.9999999999999716, -20.00000000000000000, -219.8500000000001080 ) ) ;
#6847 = VECTOR ( 'NONE', #9856, 1000.000000000000000 ) ;
#6848 = EDGE_CURVE ( 'NONE', #4302, #9549, #12174, .T. ) ;
#6849 = FACE_OUTER_BOUND ( 'NONE', #12992, .T. ) ;
#6850 = CARTESIAN_POINT ( 'NONE',  ( 3.999999999999998224, 2.472263674411418588, -3.687027874309861897 ) ) ;
#6851 = CARTESIAN_POINT ( 'NONE',  ( 134.9999999999999432, -36.99999999999997868, -180.0000000000000000 ) ) ;
#6852 = DIRECTION ( 'NONE',  ( -0.000000000000000000, 1.000000000000000000, -0.000000000000000000 ) ) ;
#6853 = ORIENTED_EDGE ( 'NONE', *, *, #2637, .T. ) ;
#6854 = CIRCLE ( 'NONE', #6845, 2.649999999999985700 ) ;
#6855 = DIRECTION ( 'NONE',  ( 1.000000000000000000, 0.000000000000000000, 0.000000000000000000 ) ) ;
#6856 = DIRECTION ( 'NONE',  ( 0.000000000000000000, 1.000000000000000000, 0.000000000000000000 ) ) ;
#6857 = EDGE_CURVE ( 'NONE', #13709, #1872, #12639, .T. ) ;
#6858 = DIRECTION ( 'NONE',  ( 0.000000000000000000, -3.606821995490527259E-15, 1.000000000000000000 ) ) ;
#6859 = EDGE_LOOP ( 'NONE', ( #12790, #12781, #7038, #12421, #4075, #9134, #6528, #9065, #10367, #10082, #1906, #9757 ) ) ;
#6860 = CIRCLE ( 'NONE', #3610, 2.649999999999985700 ) ;
#6861 = DIRECTION ( 'NONE',  ( 1.000000000000000000, 0.000000000000000000, 0.000000000000000000 ) ) ;
#6862 = AXIS2_PLACEMENT_3D ( 'NONE', #12291, #5412, #3313 ) ;
#6863 = CARTESIAN_POINT ( 'NONE',  ( 2.500000000000000000, -1.768423874527823569, 1.021000000000002350 ) ) ;
#6864 = DIRECTION ( 'NONE',  ( 0.000000000000000000, 0.000000000000000000, 1.000000000000000000 ) ) ;
#6865 = VECTOR ( 'NONE', #12133, 1000.000000000000000 ) ;
#6866 = ORIENTED_EDGE ( 'NONE', *, *, #9534, .F. ) ;
#6867 = TOROIDAL_SURFACE ( 'NONE', #9426, 4.000000000000000000, 0.2500000000000000000 ) ;
#6868 = LINE ( 'NONE', #13325, #2920 ) ;
#6869 = ORIENTED_EDGE ( 'NONE', *, *, #64, .T. ) ;
#6870 = FACE_OUTER_BOUND ( 'NONE', #10927, .T. ) ;
#6871 = AXIS2_PLACEMENT_3D ( 'NONE', #10766, #11927, #1973 ) ;
#6872 = AXIS2_PLACEMENT_3D ( 'NONE', #6901, #1451, #12557 ) ;
#6873 = ORIENTED_EDGE ( 'NONE', *, *, #13953, .T. ) ;
#6874 = ORIENTED_EDGE ( 'NONE', *, *, #2360, .T. ) ;
#6875 = PLANE ( 'NONE',  #7313 ) ;
#6876 = CARTESIAN_POINT ( 'NONE',  ( 4.235886605889389145, 2.417314728048528760, -3.751161874094018245 ) ) ;
#6877 = CIRCLE ( 'NONE', #12219, 2.649999999999985700 ) ;
#6878 = FACE_OUTER_BOUND ( 'NONE', #2546, .T. ) ;
#6879 = CARTESIAN_POINT ( 'NONE',  ( 8.000000000000000000, -4.896755294805453861E-15, 0.5150000000000000133 ) ) ;
#6880 = CIRCLE ( 'NONE', #7111, 12.00000000000000000 ) ;
#6881 = DIRECTION ( 'NONE',  ( 0.000000000000000000, -1.000000000000000000, 1.287488025362403787E-15 ) ) ;
#6882 = DIRECTION ( 'NONE',  ( -1.000000000000000000, 0.000000000000000000, 0.000000000000000000 ) ) ;
#6883 =( LENGTH_UNIT ( ) NAMED_UNIT ( * ) SI_UNIT ( .MILLI., .METRE. ) );
#6884 = CYLINDRICAL_SURFACE ( 'NONE', #12950, 2.500000000000002220 ) ;
#6885 = CONTEXT_DEPENDENT_SHAPE_REPRESENTATION ( #1292, #11330 ) ;
#6886 = VECTOR ( 'NONE', #10522, 1000.000000000000000 ) ;
#6887 = CIRCLE ( 'NONE', #4349, 0.2000000000000000944 ) ;
#6888 = ORIENTED_EDGE ( 'NONE', *, *, #4353, .T. ) ;
#6889 = EDGE_CURVE ( 'NONE', #9466, #6489, #795, .T. ) ;
#6890 = ORIENTED_EDGE ( 'NONE', *, *, #12428, .F. ) ;
#6891 = DIRECTION ( 'NONE',  ( -0.000000000000000000, -0.000000000000000000, -1.000000000000000000 ) ) ;
#6892 = AXIS2_PLACEMENT_3D ( 'NONE', #13278, #9811, #6467 ) ;
#6893 = ORIENTED_EDGE ( 'NONE', *, *, #12397, .T. ) ;
#6894 = CARTESIAN_POINT ( 'NONE',  ( 0.000000000000000000, 2.357898499370433054, -1.951563910473907981E-15 ) ) ;
#6895 = AXIS2_PLACEMENT_3D ( 'NONE', #6811, #44, #11313 ) ;
#6896 = ORIENTED_EDGE ( 'NONE', *, *, #9416, .F. ) ;
#6897 = DIRECTION ( 'NONE',  ( 0.000000000000000000, 0.000000000000000000, 1.000000000000000000 ) ) ;
#6898 = ORIENTED_EDGE ( 'NONE', *, *, #11104, .T. ) ;
#6899 = DIRECTION ( 'NONE',  ( -0.000000000000000000, -1.000000000000000000, -0.000000000000000000 ) ) ;
#6900 =( GEOMETRIC_REPRESENTATION_CONTEXT ( 3 ) GLOBAL_UNCERTAINTY_ASSIGNED_CONTEXT ( ( #6189 ) ) GLOBAL_UNIT_ASSIGNED_CONTEXT ( ( #13673, #9399, #2804 ) ) REPRESENTATION_CONTEXT ( 'NONE', 'WORKASPACE' ) );
#6901 = CARTESIAN_POINT ( 'NONE',  ( 140.0000000000000000, -75.00000000000008527, 190.0000000000000000 ) ) ;
#6902 = LINE ( 'NONE', #2478, #5720 ) ;
#6903 = DIRECTION ( 'NONE',  ( -0.000000000000000000, 1.000000000000000000, -0.000000000000000000 ) ) ;
#6904 = CARTESIAN_POINT ( 'NONE',  ( 140.0000000000000000, -95.00000000000008527, 190.0000000000000000 ) ) ;
#6905 = CARTESIAN_POINT ( 'NONE',  ( 134.9999999999999432, -36.99999999999997868, -169.9999999999999716 ) ) ;
#6906 = EDGE_LOOP ( 'NONE', ( #6201, #13009, #1132, #11532 ) ) ;
#6907 = PRESENTATION_LAYER_ASSIGNMENT (  '', '', ( #10149 ) ) ;
#6908 = EDGE_LOOP ( 'NONE', ( #2780, #6866, #7688, #11826, #408, #5184, #7968, #8995 ) ) ;
#6909 = ORIENTED_EDGE ( 'NONE', *, *, #11653, .F. ) ;
#6910 = FACE_OUTER_BOUND ( 'NONE', #11822, .T. ) ;
#6911 = ORIENTED_EDGE ( 'NONE', *, *, #7618, .T. ) ;
#6912 = CARTESIAN_POINT ( 'NONE',  ( -299.9999999999999432, -95.00000000000008527, 39.99999999999997868 ) ) ;
#6913 = VERTEX_POINT ( 'NONE', #10236 ) ;
#6914 = EDGE_CURVE ( 'NONE', #11936, #13138, #1034, .T. ) ;
#6915 = DIRECTION ( 'NONE',  ( -0.000000000000000000, 1.000000000000000000, 0.000000000000000000 ) ) ;
#6916 = ADVANCED_FACE ( 'NONE', ( #9006, #4734 ), #7971, .F. ) ;
#6917 = DIRECTION ( 'NONE',  ( 0.000000000000000000, 0.000000000000000000, 1.000000000000000000 ) ) ;
#6918 = CARTESIAN_POINT ( 'NONE',  ( -222.6499999999998920, -85.00000000000009948, 30.00000000000000000 ) ) ;
#6919 = DIRECTION ( 'NONE',  ( 0.000000000000000000, 0.000000000000000000, -1.000000000000000000 ) ) ;
#6920 = AXIS2_PLACEMENT_3D ( 'NONE', #13908, #1718, #3120 ) ;
#6921 = CARTESIAN_POINT ( 'NONE',  ( 142.6500000000000057, -75.00000000000008527, -190.0000000000000000 ) ) ;
#6922 = PRODUCT ( 'hex flange nut gradea_iso_ISO - 4161 - M5 - N', 'hex flange nut gradea_iso_ISO - 4161 - M5 - N', '', ( #6977 ) ) ;
#6923 = FACE_BOUND ( 'NONE', #4235, .T. ) ;
#6924 = ADVANCED_FACE ( 'NONE', ( #8048 ), #1231, .F. ) ;
#6925 = VERTEX_POINT ( 'NONE', #58 ) ;
#6926 = CARTESIAN_POINT ( 'NONE',  ( 1.317756351988342622, -3.857995168970215438, -0.04852650426602527628 ) ) ;
#6927 = AXIS2_PLACEMENT_3D ( 'NONE', #8227, #13749, #4917 ) ;
#6928 = EDGE_CURVE ( 'NONE', #32, #10282, #1274, .T. ) ;
#6929 = DIRECTION ( 'NONE',  ( 1.000000000000000000, 0.000000000000000000, 0.000000000000000000 ) ) ;
#6930 = CARTESIAN_POINT ( 'NONE',  ( 1.411581201560190495E-15, 4.862606272033091592, -3.745885042887436622 ) ) ;
#6931 = ORIENTED_EDGE ( 'NONE', *, *, #13208, .F. ) ;
#6932 = PLANE ( 'NONE',  #5707 ) ;
#6933 = CARTESIAN_POINT ( 'NONE',  ( 219.9999999999999716, -85.00000000000007105, 55.00000000000002132 ) ) ;
#6934 = DIRECTION ( 'NONE',  ( 6.123233995736766036E-17, -1.000000000000000000, 0.000000000000000000 ) ) ;
#6935 = AXIS2_PLACEMENT_3D ( 'NONE', #224, #4902, #9104 ) ;
#6936 = EDGE_CURVE ( 'NONE', #3581, #4585, #269, .T. ) ;
#6937 = ADVANCED_FACE ( 'NONE', ( #10093 ), #1160, .F. ) ;
#6938 = EDGE_CURVE ( 'NONE', #10282, #32, #5917, .T. ) ;
#6939 = EDGE_CURVE ( 'NONE', #8960, #3920, #3166, .T. ) ;
#6940 = VERTEX_POINT ( 'NONE', #11255 ) ;
#6941 = FACE_OUTER_BOUND ( 'NONE', #2873, .T. ) ;
#6942 = EDGE_LOOP ( 'NONE', ( #8407, #9013, #10337, #10470 ) ) ;
#6943 = DIRECTION ( 'NONE',  ( -1.000000000000000000, -1.460819769243627131E-16, 0.000000000000000000 ) ) ;
#6944 = ADVANCED_FACE ( 'NONE', ( #10034 ), #9144, .F. ) ;
#6945 = EDGE_LOOP ( 'NONE', ( #2076, #8794, #5225, #10011 ) ) ;
#6946 = ORIENTED_EDGE ( 'NONE', *, *, #10540, .T. ) ;
#6947 = LINE ( 'NONE', #12538, #6407 ) ;
#6948 = CARTESIAN_POINT ( 'NONE',  ( 0.5636800770130377947, 4.293361309317166530, -3.531542292954102713 ) ) ;
#6949 = CIRCLE ( 'NONE', #11825, 13.50000000000000178 ) ;
#6950 = CARTESIAN_POINT ( 'NONE',  ( 0.000000000000000000, 0.000000000000000000, -4.974599999999998801 ) ) ;
#6951 = CARTESIAN_POINT ( 'NONE',  ( 2.500000000000000000, 2.500728763858895382E-16, -2.041999999999999815 ) ) ;
#6952 = DIRECTION ( 'NONE',  ( -0.000000000000000000, -0.000000000000000000, -1.000000000000000000 ) ) ;
#6953 = DIRECTION ( 'NONE',  ( -1.000000000000000000, -0.000000000000000000, -0.000000000000000000 ) ) ;
#6954 =( NAMED_UNIT ( * ) SI_UNIT ( $, .STERADIAN. ) SOLID_ANGLE_UNIT ( ) );
#6955 = AXIS2_PLACEMENT_3D ( 'NONE', #6639, #9025, #9102 ) ;
#6956 = DIRECTION ( 'NONE',  ( 1.000000000000000000, 0.000000000000000000, 0.000000000000000000 ) ) ;
#6957 = ORIENTED_EDGE ( 'NONE', *, *, #13180, .T. ) ;
#6958 = ADVANCED_BREP_SHAPE_REPRESENTATION ( '', ( #3823, #14039 ), #4938 ) ;
#6959 = EDGE_LOOP ( 'NONE', ( #6362, #3956 ) ) ;
#6960 = DIRECTION ( 'NONE',  ( -0.000000000000000000, -0.000000000000000000, 1.000000000000000000 ) ) ;
#6961 = CIRCLE ( 'NONE', #1629, 2.649999999999985700 ) ;
#6962 =( REPRESENTATION_RELATIONSHIP ('NONE','NONE', #11251, #208 ) REPRESENTATION_RELATIONSHIP_WITH_TRANSFORMATION ( #13338 )SHAPE_REPRESENTATION_RELATIONSHIP( ) );
#6963 = ORIENTED_EDGE ( 'NONE', *, *, #9972, .F. ) ;
#6964 = FACE_OUTER_BOUND ( 'NONE', #4630, .T. ) ;
#6965 = EDGE_LOOP ( 'NONE', ( #9396, #1749, #7008 ) ) ;
#6966 = LINE ( 'NONE', #8118, #4806 ) ;
#6967 = ORIENTED_EDGE ( 'NONE', *, *, #11890, .F. ) ;
#6968 = AXIS2_PLACEMENT_3D ( 'NONE', #9390, #3876, #12435 ) ;
#6969 = CARTESIAN_POINT ( 'NONE',  ( 1.849560077140108394, 0.7556913915602446741, 0.5149999999999996803 ) ) ;
#6970 = CARTESIAN_POINT ( 'NONE',  ( 136.6666666666666288, -25.00000000000000000, -225.1500000000000625 ) ) ;
#6971 = ORIENTED_EDGE ( 'NONE', *, *, #1803, .F. ) ;
#6972 = DIRECTION ( 'NONE',  ( -1.000000000000000000, -0.000000000000000000, -0.000000000000000000 ) ) ;
#6973 = EDGE_CURVE ( 'NONE', #7848, #5316, #10164, .T. ) ;
#6974 = CARTESIAN_POINT ( 'NONE',  ( -25.39999999999996305, 0.000000000000000000, 0.000000000000000000 ) ) ;
#6975 = CIRCLE ( 'NONE', #695, 2.055000000000000160 ) ;
#6976 =( NAMED_UNIT ( * ) SI_UNIT ( $, .STERADIAN. ) SOLID_ANGLE_UNIT ( ) );
#6977 = PRODUCT_CONTEXT ( 'NONE', #10074, 'mechanical' ) ;
#6978 = CARTESIAN_POINT ( 'NONE',  ( 2.500000000000000000, -1.178949249685213863, 2.042000000000002924 ) ) ;
#6979 = VERTEX_POINT ( 'NONE', #200 ) ;
#6980 = ORIENTED_EDGE ( 'NONE', *, *, #5366, .T. ) ;
#6981 = VERTEX_POINT ( 'NONE', #3635 ) ;
#6982 = LINE ( 'NONE', #5559, #10672 ) ;
#6983 = VECTOR ( 'NONE', #10260, 1000.000000000000000 ) ;
#6984 = VERTEX_POINT ( 'NONE', #7766 ) ;
#6985 = CARTESIAN_POINT ( 'NONE',  ( 0.7826237921249276086, 1.524685264938454646E-15, -12.44999999999999929 ) ) ;
#6986 = ORIENTED_EDGE ( 'NONE', *, *, #8605, .F. ) ;
#6987 = DIRECTION ( 'NONE',  ( 0.000000000000000000, 0.000000000000000000, -1.000000000000000000 ) ) ;
#6988 = STYLED_ITEM ( 'NONE', ( #9280 ), #5258 ) ;
#6989 = EDGE_CURVE ( 'NONE', #12864, #4316, #808, .T. ) ;
#6990 = CARTESIAN_POINT ( 'NONE',  ( 5.000000000000004441, 0.000000000000000000, 0.000000000000000000 ) ) ;
#6991 = CARTESIAN_POINT ( 'NONE',  ( -6.259644161404860030E-16, -4.618802153517027165, -5.000000000000000000 ) ) ;
#6992 = CARTESIAN_POINT ( 'NONE',  ( -1.800000000000002931, 0.000000000000000000, 0.000000000000000000 ) ) ;
#6993 = DIRECTION ( 'NONE',  ( 1.000000000000000000, 0.000000000000000000, 0.000000000000000000 ) ) ;
#6994 = DIRECTION ( 'NONE',  ( -0.000000000000000000, -0.000000000000000000, 1.000000000000000000 ) ) ;
#6995 = CIRCLE ( 'NONE', #7684, 11.05000000000000071 ) ;
#6996 = FACE_OUTER_BOUND ( 'NONE', #6709, .T. ) ;
#6997 = EDGE_CURVE ( 'NONE', #12847, #8809, #7771, .T. ) ;
#6998 = ORIENTED_EDGE ( 'NONE', *, *, #6614, .T. ) ;
#6999 = AXIS2_PLACEMENT_3D ( 'NONE', #3605, #11368, #1341 ) ;
#7000 =( GEOMETRIC_REPRESENTATION_CONTEXT ( 3 ) GLOBAL_UNCERTAINTY_ASSIGNED_CONTEXT ( ( #14085 ) ) GLOBAL_UNIT_ASSIGNED_CONTEXT ( ( #5987, #439, #9327 ) ) REPRESENTATION_CONTEXT ( 'NONE', 'WORKASPACE' ) );
#7001 = VECTOR ( 'NONE', #5320, 1000.000000000000000 ) ;
#7002 =( NAMED_UNIT ( * ) PLANE_ANGLE_UNIT ( ) SI_UNIT ( $, .RADIAN. ) );
#7003 = CARTESIAN_POINT ( 'NONE',  ( 299.9999999999999432, -75.00000000000008527, 190.0000000000000000 ) ) ;
#7004 = FACE_OUTER_BOUND ( 'NONE', #4237, .T. ) ;
#7005 = AXIS2_PLACEMENT_3D ( 'NONE', #10360, #4931, #9494 ) ;
#7006 = SURFACE_STYLE_USAGE ( .BOTH. , #2585 ) ;
#7007 = ORIENTED_EDGE ( 'NONE', *, *, #14207, .F. ) ;
#7008 = ORIENTED_EDGE ( 'NONE', *, *, #5092, .T. ) ;
#7009 = STYLED_ITEM ( 'NONE', ( #2556 ), #12151 ) ;
#7010 = FACE_OUTER_BOUND ( 'NONE', #4920, .T. ) ;
#7011 = AXIS2_PLACEMENT_3D ( 'NONE', #550, #8186, #11753 ) ;
#7012 = DIRECTION ( 'NONE',  ( -0.8660254037844373753, 0.5000000000000021094, 0.000000000000000000 ) ) ;
#7013 = DIRECTION ( 'NONE',  ( 1.000000000000000000, 0.000000000000000000, 0.000000000000000000 ) ) ;
#7014 = EDGE_CURVE ( 'NONE', #6255, #1625, #4662, .T. ) ;
#7015 = CARTESIAN_POINT ( 'NONE',  ( 299.9999999999999432, -95.00000000000008527, 190.0000000000000000 ) ) ;
#7016 = ADVANCED_FACE ( 'NONE', ( #12200 ), #12276, .F. ) ;
#7017 = ORIENTED_EDGE ( 'NONE', *, *, #3061, .F. ) ;
#7018 = DIRECTION ( 'NONE',  ( 0.000000000000000000, 0.000000000000000000, 1.000000000000000000 ) ) ;
#7019 = DIRECTION ( 'NONE',  ( 1.000000000000000000, 0.000000000000000000, -0.000000000000000000 ) ) ;
#7020 = DIRECTION ( 'NONE',  ( -0.000000000000000000, -0.000000000000000000, -1.000000000000000000 ) ) ;
#7021 = EDGE_LOOP ( 'NONE', ( #4262, #12371 ) ) ;
#7022 = DIRECTION ( 'NONE',  ( 0.000000000000000000, 1.000000000000000000, 0.000000000000000000 ) ) ;
#7023 = EDGE_CURVE ( 'NONE', #9740, #5927, #8461, .T. ) ;
#7024 = EDGE_CURVE ( 'NONE', #4150, #8111, #12409, .T. ) ;
#7025 = LINE ( 'NONE', #13533, #7781 ) ;
#7026 = CYLINDRICAL_SURFACE ( 'NONE', #1557, 2.649999999999985700 ) ;
#7027 = EDGE_CURVE ( 'NONE', #5131, #9938, #635, .T. ) ;
#7028 = FACE_OUTER_BOUND ( 'NONE', #8917, .T. ) ;
#7029 = CARTESIAN_POINT ( 'NONE',  ( 305.4999999999999432, -75.00000000000008527, -190.0000000000000000 ) ) ;
#7030 = DIRECTION ( 'NONE',  ( 0.000000000000000000, 0.000000000000000000, 1.000000000000000000 ) ) ;
#7031 = CYLINDRICAL_SURFACE ( 'NONE', #9005, 2.500000000000002220 ) ;
#7032 = ITEM_DEFINED_TRANSFORMATION ( 'NONE', 'NONE', #2831,  #14039 ) ;
#7033 = ORIENTED_EDGE ( 'NONE', *, *, #10587, .F. ) ;
#7034 = VERTEX_POINT ( 'NONE', #1732 ) ;
#7035 = DIRECTION ( 'NONE',  ( -0.000000000000000000, -0.000000000000000000, 1.000000000000000000 ) ) ;
#7036 = ORIENTED_EDGE ( 'NONE', *, *, #13724, .F. ) ;
#7037 = DIRECTION ( 'NONE',  ( 0.000000000000000000, 0.000000000000000000, 1.000000000000000000 ) ) ;
#7038 = ORIENTED_EDGE ( 'NONE', *, *, #13435, .F. ) ;
#7039 = CYLINDRICAL_SURFACE ( 'NONE', #8968, 2.649999999999985700 ) ;
#7040 = ORIENTED_EDGE ( 'NONE', *, *, #2443, .F. ) ;
#7041 = CARTESIAN_POINT ( 'NONE',  ( 0.06760930072668806801, -4.837354856632045452E-15, 0.000000000000000000 ) ) ;
#7042 = PRODUCT_DEFINITION_SHAPE ( 'NONE', 'NONE',  #75 ) ;
#7043 = PLANE ( 'NONE',  #11068 ) ;
#7044 = ORIENTED_EDGE ( 'NONE', *, *, #13071, .F. ) ;
#7045 = CYLINDRICAL_SURFACE ( 'NONE', #12952, 2.500000000000000444 ) ;
#7046 = SURFACE_STYLE_FILL_AREA ( #8196 ) ;
#7047 =( LENGTH_UNIT ( ) NAMED_UNIT ( * ) SI_UNIT ( .MILLI., .METRE. ) );
#7048 = SHAPE_DEFINITION_REPRESENTATION ( #12247, #10796 ) ;
#7049 = FACE_OUTER_BOUND ( 'NONE', #12196, .T. ) ;
#7050 = ORIENTED_EDGE ( 'NONE', *, *, #10635, .T. ) ;
#7051 = ORIENTED_EDGE ( 'NONE', *, *, #6144, .T. ) ;
#7052 = VERTEX_POINT ( 'NONE', #10301 ) ;
#7053 = ADVANCED_FACE ( 'NONE', ( #2839 ), #13797, .T. ) ;
#7054 = CARTESIAN_POINT ( 'NONE',  ( 0.000000000000000000, 0.000000000000000000, 55.00000000000001421 ) ) ;
#7055 = ORIENTED_EDGE ( 'NONE', *, *, #12154, .T. ) ;
#7056 = CARTESIAN_POINT ( 'NONE',  ( 10.00000000000000000, 1.224646799147353256E-15, 200.0000000000000000 ) ) ;
#7057 = ORIENTED_EDGE ( 'NONE', *, *, #10321, .F. ) ;
#7058 = DIRECTION ( 'NONE',  ( -0.000000000000000000, -0.000000000000000000, -1.000000000000000000 ) ) ;
#7059 = DIRECTION ( 'NONE',  ( 1.000000000000000000, 0.000000000000000000, 0.000000000000000000 ) ) ;
#7060 = DIRECTION ( 'NONE',  ( -1.000000000000000000, 0.000000000000000000, 0.000000000000000000 ) ) ;
#7061 = AXIS2_PLACEMENT_3D ( 'NONE', #7691, #7759, #8649 ) ;
#7062 = CARTESIAN_POINT ( 'NONE',  ( 53.33333333333330017, -20.00000000000000000, 225.1500000000000625 ) ) ;
#7063 = AXIS2_PLACEMENT_3D ( 'NONE', #11217, #9028, #2578 ) ;
#7064 = CARTESIAN_POINT ( 'NONE',  ( 140.0000000000000000, -95.00000000000008527, 190.0000000000000000 ) ) ;
#7065 = CARTESIAN_POINT ( 'NONE',  ( -30.00000000000002842, -20.00000000000000000, 250.0000000000000000 ) ) ;
#7066 = DIRECTION ( 'NONE',  ( -0.000000000000000000, -0.000000000000000000, -1.000000000000000000 ) ) ;
#7067 = ORIENTED_EDGE ( 'NONE', *, *, #13403, .T. ) ;
#7068 = EDGE_CURVE ( 'NONE', #1365, #1312, #5952, .T. ) ;
#7069 = DIRECTION ( 'NONE',  ( 0.000000000000000000, 0.000000000000000000, -1.000000000000000000 ) ) ;
#7070 = DIRECTION ( 'NONE',  ( 1.000000000000000000, 0.000000000000000000, 0.000000000000000000 ) ) ;
#7071 = CYLINDRICAL_SURFACE ( 'NONE', #13374, 5.000000000000004441 ) ;
#7072 = ORIENTED_EDGE ( 'NONE', *, *, #13006, .T. ) ;
#7073 = EDGE_CURVE ( 'NONE', #13284, #10673, #7179, .T. ) ;
#7074 = CARTESIAN_POINT ( 'NONE',  ( 2.740000000000000213, -0.5150000000000034550, 0.9838866223909985553 ) ) ;
#7075 = AXIS2_PLACEMENT_3D ( 'NONE', #5098, #556, #10451 ) ;
#7076 = CARTESIAN_POINT ( 'NONE',  ( 2.500000000000000000, 1.768423874527823791, 1.020999999999998353 ) ) ;
#7077 = CARTESIAN_POINT ( 'NONE',  ( 219.9999999999999716, -10.00000000000000000, -222.5000000000000853 ) ) ;
#7078 = CARTESIAN_POINT ( 'NONE',  ( 219.9999999999999716, -85.00000000000007105, 0.000000000000000000 ) ) ;
#7079 = ORIENTED_EDGE ( 'NONE', *, *, #704, .T. ) ;
#7080 = PLANE ( 'NONE',  #10424 ) ;
#7081 = DIRECTION ( 'NONE',  ( -0.000000000000000000, 1.000000000000000000, -0.000000000000000000 ) ) ;
#7082 = VERTEX_POINT ( 'NONE', #7109 ) ;
#7084 = ADVANCED_FACE ( 'NONE', ( #1584 ), #11610, .F. ) ;
#7083 = FACE_BOUND ( 'NONE', #7493, .T. ) ;
#7085 = CIRCLE ( 'NONE', #5973, 5.500000000000005329 ) ;
#7086 = DIRECTION ( 'NONE',  ( -1.000000000000000000, 0.000000000000000000, 0.000000000000000000 ) ) ;
#7087 = EDGE_CURVE ( 'NONE', #2907, #13843, #3391, .T. ) ;
#7088 = DIRECTION ( 'NONE',  ( 0.000000000000000000, 1.000000000000000000, -1.471414886128461471E-15 ) ) ;
#7089 = CARTESIAN_POINT ( 'NONE',  ( 5.000000000000004441, 5.204748896376250699E-16, -4.250000000000000000 ) ) ;
#7090 = DIRECTION ( 'NONE',  ( 0.000000000000000000, 1.000000000000000000, 0.000000000000000000 ) ) ;
#7091 = DIRECTION ( 'NONE',  ( 0.000000000000000000, -0.8660254037844390407, -0.4999999999999993339 ) ) ;
#7092 = CIRCLE ( 'NONE', #10574, 7.983406227920510467 ) ;
#7093 = EDGE_CURVE ( 'NONE', #7302, #4565, #6395, .T. ) ;
#7094 = FACE_OUTER_BOUND ( 'NONE', #13429, .T. ) ;
#7095 = CIRCLE ( 'NONE', #4829, 2.500000000000000444 ) ;
#7096 = VECTOR ( 'NONE', #7022, 1000.000000000000000 ) ;
#7097 = EDGE_LOOP ( 'NONE', ( #8330, #8023, #13248 ) ) ;
#7098 = VERTEX_POINT ( 'NONE', #8338 ) ;
#7099 = EDGE_CURVE ( 'NONE', #8115, #2239, #6167, .T. ) ;
#7100 = CIRCLE ( 'NONE', #13116, 10.20000000000000107 ) ;
#7101 = FACE_OUTER_BOUND ( 'NONE', #772, .T. ) ;
#7102 = VERTEX_POINT ( 'NONE', #13706 ) ;
#7103 = CARTESIAN_POINT ( 'NONE',  ( 0.000000000000000000, -8.660254037844389075, 200.0000000000000000 ) ) ;
#7104 = CARTESIAN_POINT ( 'NONE',  ( 347.0000000000000000, -8.660254037844389075, 200.0000000000000000 ) ) ;
#7105 = CIRCLE ( 'NONE', #6648, 5.000000000000004441 ) ;
#7106 = ORIENTED_EDGE ( 'NONE', *, *, #10859, .F. ) ;
#7107 = FACE_OUTER_BOUND ( 'NONE', #6240, .T. ) ;
#7108 = ORIENTED_EDGE ( 'NONE', *, *, #13504, .F. ) ;
#7110 = ADVANCED_FACE ( 'NONE', ( #3996 ), #1449, .F. ) ;
#7109 = CARTESIAN_POINT ( 'NONE',  ( 5.000000000000002665, 0.000000000000000000, -2.700000000000000622 ) ) ;
#7111 = AXIS2_PLACEMENT_3D ( 'NONE', #1537, #2866, #8210 ) ;
#7112 = CARTESIAN_POINT ( 'NONE',  ( 2.500000000000000000, 2.357898499370433054, -1.951563910473907981E-15 ) ) ;
#7113 = VERTEX_POINT ( 'NONE', #9511 ) ;
#7114 = PRODUCT_DEFINITION_CONTEXT ( 'detailed design', #3874, 'design' ) ;
#7115 =( NAMED_UNIT ( * ) SI_UNIT ( $, .STERADIAN. ) SOLID_ANGLE_UNIT ( ) );
#7116 = VECTOR ( 'NONE', #423, 1000.000000000000000 ) ;
#7117 = DIRECTION ( 'NONE',  ( -1.000000000000000000, -0.000000000000000000, -0.000000000000000000 ) ) ;
#7118 = AXIS2_PLACEMENT_3D ( 'NONE', #5460, #11054, #6827 ) ;
#7119 = DIRECTION ( 'NONE',  ( 0.000000000000000000, 0.000000000000000000, 1.000000000000000000 ) ) ;
#7120 = APPLICATION_PROTOCOL_DEFINITION ( 'draft international standard', 'automotive_design', 1998, #11106 ) ;
#7121 = CARTESIAN_POINT ( 'NONE',  ( -1.999999999999999556, 3.464101615137754830, -3.142992957459232795 ) ) ;
#7122 = VECTOR ( 'NONE', #5746, 1000.000000000000000 ) ;
#7123 = ORIENTED_EDGE ( 'NONE', *, *, #6172, .T. ) ;
#7124 = EDGE_CURVE ( 'NONE', #5874, #3993, #8410, .T. ) ;
#7125 = DIRECTION ( 'NONE',  ( 0.000000000000000000, 0.000000000000000000, -1.000000000000000000 ) ) ;
#7126 = AXIS2_PLACEMENT_3D ( 'NONE', #11170, #1214, #250 ) ;
#7127 = ORIENTED_EDGE ( 'NONE', *, *, #7366, .F. ) ;
#7128 = ADVANCED_FACE ( 'NONE', ( #2692 ), #483, .F. ) ;
#7129 = CARTESIAN_POINT ( 'NONE',  ( -294.9999999999999432, 55.00000000000001421, 40.00000000000000000 ) ) ;
#7130 = COLOUR_RGB ( '',1.000000000000000000, 0.9490196078431372140, 0.9098039215686274384 ) ;
#7131 = ORIENTED_EDGE ( 'NONE', *, *, #9072, .T. ) ;
#7132 = CARTESIAN_POINT ( 'NONE',  ( 2.500000000000000000, 1.768423874527822681, -1.021000000000002794 ) ) ;
#7133 = ORIENTED_EDGE ( 'NONE', *, *, #2242, .T. ) ;
#7134 = CARTESIAN_POINT ( 'NONE',  ( 25.00000000000000000, 0.000000000000000000, 2.055000000000000160 ) ) ;
#7135 = EDGE_CURVE ( 'NONE', #8981, #8755, #7267, .T. ) ;
#7136 = FILL_AREA_STYLE_COLOUR ( '', #3899 ) ;
#7137 = FACE_BOUND ( 'NONE', #13938, .T. ) ;
#7138 = CARTESIAN_POINT ( 'NONE',  ( 134.9999999999999432, -56.99999999999997158, -180.0000000000000000 ) ) ;
#7139 = DIRECTION ( 'NONE',  ( -0.000000000000000000, -0.000000000000000000, -1.000000000000000000 ) ) ;
#7140 = DIRECTION ( 'NONE',  ( -0.000000000000000000, -0.000000000000000000, 1.000000000000000000 ) ) ;
#7141 = EDGE_LOOP ( 'NONE', ( #14199, #9842, #10248, #11411 ) ) ;
#7142 = ORIENTED_EDGE ( 'NONE', *, *, #4470, .T. ) ;
#7143 = ORIENTED_EDGE ( 'NONE', *, *, #4985, .T. ) ;
#7144 = CARTESIAN_POINT ( 'NONE',  ( 2.500000000000000000, -1.178949249685213863, 2.042000000000002924 ) ) ;
#7145 = FACE_OUTER_BOUND ( 'NONE', #11095, .T. ) ;
#7146 = FILL_AREA_STYLE ('',( #8222 ) ) ;
#7147 = ORIENTED_EDGE ( 'NONE', *, *, #7593, .F. ) ;
#7148 = AXIS2_PLACEMENT_3D ( 'NONE', #8396, #9718, #12827 ) ;
#7149 = DIRECTION ( 'NONE',  ( 1.000000000000000000, 0.000000000000000000, 0.000000000000000000 ) ) ;
#7150 = EDGE_CURVE ( 'NONE', #5386, #4689, #9439, .T. ) ;
#7151 = DIRECTION ( 'NONE',  ( -0.000000000000000000, 0.000000000000000000, 1.000000000000000000 ) ) ;
#7152 = DIRECTION ( 'NONE',  ( 0.000000000000000000, 0.000000000000000000, -1.000000000000000000 ) ) ;
#7153 = DIRECTION ( 'NONE',  ( -0.000000000000000000, -0.000000000000000000, 1.000000000000000000 ) ) ;
#7154 = DIRECTION ( 'NONE',  ( 0.000000000000000000, -0.000000000000000000, -1.000000000000000000 ) ) ;
#7155 = ORIENTED_EDGE ( 'NONE', *, *, #11156, .F. ) ;
#7156 = CARTESIAN_POINT ( 'NONE',  ( 219.9999999999999716, -25.00000000000000000, -222.5000000000000853 ) ) ;
#7157 = DIRECTION ( 'NONE',  ( -0.000000000000000000, 1.000000000000000000, -0.000000000000000000 ) ) ;
#7158 = EDGE_LOOP ( 'NONE', ( #988, #11180, #10482, #8479 ) ) ;
#7159 = EDGE_CURVE ( 'NONE', #11362, #8755, #9412, .T. ) ;
#7160 = LINE ( 'NONE', #4781, #5513 ) ;
#7161 = CIRCLE ( 'NONE', #5558, 4.556291390728477886 ) ;
#7162 = LINE ( 'NONE', #12750, #10679 ) ;
#7163 = LINE ( 'NONE', #11594, #11175 ) ;
#7164 = DIRECTION ( 'NONE',  ( -1.000000000000000000, 0.000000000000000000, 0.000000000000000000 ) ) ;
#7165 = VECTOR ( 'NONE', #3324, 1000.000000000000000 ) ;
#7166 = CARTESIAN_POINT ( 'NONE',  ( 3.900000000000000799, 0.000000000000000000, 0.000000000000000000 ) ) ;
#7167 = VERTEX_POINT ( 'NONE', #1659 ) ;
#7168 = ADVANCED_FACE ( 'NONE', ( #13853 ), #11400, .F. ) ;
#7169 = DIRECTION ( 'NONE',  ( 0.000000000000000000, 0.000000000000000000, 1.000000000000000000 ) ) ;
#7170 = EDGE_CURVE ( 'NONE', #1051, #13286, #12556, .T. ) ;
#7171 = VERTEX_POINT ( 'NONE', #10816 ) ;
#7172 = DIRECTION ( 'NONE',  ( -1.000000000000000000, 0.000000000000000000, 0.000000000000000000 ) ) ;
#7173 = CARTESIAN_POINT ( 'NONE',  ( 137.3500000000000227, -75.00000000000008527, -169.9999999999999716 ) ) ;
#7174 =( BOUNDED_SURFACE ( )  B_SPLINE_SURFACE ( 3, 2, ( 
 ( #985, #5434, #9858 ),
 ( #12319, #13529, #7948 ),
 ( #3476, #4497, #10211 ),
 ( #10142, #11308, #7877 ),
 ( #9121, #13464, #4712 ),
 ( #38, #243, #4634 ) ),
 .UNSPECIFIED., .F., .F., .T. ) 
 B_SPLINE_SURFACE_WITH_KNOTS ( ( 4, 2, 4 ),
 ( 3, 3 ),
 ( 0.02032853247518126918, 0.02278863295364821906, 0.02524873343211517240 ),
 ( 0.000000000000000000, 1.000000000000000000 ),
 .UNSPECIFIED. ) 
 GEOMETRIC_REPRESENTATION_ITEM ( )  RATIONAL_B_SPLINE_SURFACE ( (
 ( 1.000000000000000000, 0.8047781615896837382, 1.000000000000000000),
 ( 1.000000000000000000, 0.8123767586289252218, 1.000000000000000000),
 ( 1.000000000000000000, 0.8190662415564388121, 1.000000000000000000),
 ( 1.000000000000000000, 0.8192361015669026303, 1.000000000000000000),
 ( 1.000000000000000000, 0.8126135807103900266, 1.000000000000000000),
 ( 1.000000000000000000, 0.8047712338318593339, 1.000000000000000000) ) ) 
 REPRESENTATION_ITEM ( '' )  SURFACE ( )  );
#7175 = VERTEX_POINT ( 'NONE', #5309 ) ;
#7176 = CARTESIAN_POINT ( 'NONE',  ( 140.0000000000000000, -95.00000000000008527, -169.9999999999999716 ) ) ;
#7177 = EDGE_LOOP ( 'NONE', ( #1096, #5732, #9899, #10046 ) ) ;
#7178 = AXIS2_PLACEMENT_3D ( 'NONE', #8476, #12908, #7395 ) ;
#7179 = LINE ( 'NONE', #7256, #9635 ) ;
#7180 = PLANE ( 'NONE',  #3881 ) ;
#7181 = ORIENTED_EDGE ( 'NONE', *, *, #12098, .F. ) ;
#7182 = DIRECTION ( 'NONE',  ( -1.000000000000000000, 0.000000000000000000, 0.000000000000000000 ) ) ;
#7183 = FILL_AREA_STYLE ('',( #10307 ) ) ;
#7184 = CARTESIAN_POINT ( 'NONE',  ( 4.999999999999999112, 8.660254037844390851, 199.9990000000000236 ) ) ;
#7185 = AXIS2_PLACEMENT_3D ( 'NONE', #8843, #9048, #13266 ) ;
#7186 = ORIENTED_EDGE ( 'NONE', *, *, #7468, .T. ) ;
#7187 = AXIS2_PLACEMENT_3D ( 'NONE', #13647, #9309, #3719 ) ;
#7188 = VERTEX_POINT ( 'NONE', #7534 ) ;
#7189 = EDGE_CURVE ( 'NONE', #3295, #5615, #576, .T. ) ;
#7190 = ORIENTED_EDGE ( 'NONE', *, *, #8242, .T. ) ;
#7191 = ADVANCED_FACE ( 'NONE', ( #13058 ), #703, .F. ) ;
#7192 = ORIENTED_EDGE ( 'NONE', *, *, #6558, .F. ) ;
#7193 = DIRECTION ( 'NONE',  ( -0.000000000000000000, -0.000000000000000000, -1.000000000000000000 ) ) ;
#7194 = EDGE_CURVE ( 'NONE', #10963, #1338, #9867, .T. ) ;
#7195 = ORIENTED_EDGE ( 'NONE', *, *, #584, .F. ) ;
#7196 = CARTESIAN_POINT ( 'NONE',  ( 359.9999999999997726, 35.00000000000002842, 10.00000000000000000 ) ) ;
#7197 = ORIENTED_EDGE ( 'NONE', *, *, #6331, .F. ) ;
#7198 = DIRECTION ( 'NONE',  ( 1.000000000000000000, 0.000000000000000000, 0.000000000000000000 ) ) ;
#7199 = UNCERTAINTY_MEASURE_WITH_UNIT (LENGTH_MEASURE( 1.000000000000000082E-05 ), #9242, 'distance_accuracy_value', 'NONE');
#7200 = AXIS2_PLACEMENT_3D ( 'NONE', #2156, #6582, #11008 ) ;
#7201 = B_SPLINE_CURVE_WITH_KNOTS ( 'NONE', 3,
 ( #6154, #4860, #13762, #13691, #2673, #1261, #1335, #3598 ),
 .UNSPECIFIED., .F., .F.,
 ( 4, 2, 2, 4 ),
 ( 2.465131517071352357E-07, 0.001183067374689843057, 0.001774477805458910071, 0.002365888236227977302 ),
 .UNSPECIFIED. ) ;
#7202 = DIRECTION ( 'NONE',  ( 0.000000000000000000, 1.000000000000000000, -1.471414886128461471E-15 ) ) ;
#7203 = ADVANCED_FACE ( 'NONE', ( #913 ), #5375, .F. ) ;
#7204 = EDGE_CURVE ( 'NONE', #5871, #14256, #6387, .T. ) ;
#7205 = DIRECTION ( 'NONE',  ( 1.000000000000000000, 0.000000000000000000, 0.000000000000000000 ) ) ;
#7206 = EDGE_CURVE ( 'NONE', #14256, #8359, #12878, .T. ) ;
#7207 = ADVANCED_FACE ( 'NONE', ( #3060, #2099 ), #9586, .T. ) ;
#7208 = VECTOR ( 'NONE', #5835, 1000.000000000000000 ) ;
#7209 = DIRECTION ( 'NONE',  ( 1.000000000000000000, 0.000000000000000000, 0.000000000000000000 ) ) ;
#7210 = CARTESIAN_POINT ( 'NONE',  ( 0.000000000000000000, -15.00000000000000000, 205.0000000000000284 ) ) ;
#7211 = ORIENTED_EDGE ( 'NONE', *, *, #11839, .T. ) ;
#7212 = VERTEX_POINT ( 'NONE', #10748 ) ;
#7213 = AXIS2_PLACEMENT_3D ( 'NONE', #9101, #9319, #3801 ) ;
#7214 = DIRECTION ( 'NONE',  ( -0.000000000000000000, 1.000000000000000000, -0.000000000000000000 ) ) ;
#7215 = PRESENTATION_LAYER_ASSIGNMENT (  '', '', ( #8373 ) ) ;
#7216 = DIRECTION ( 'NONE',  ( -0.000000000000000000, 1.000000000000000000, -0.000000000000000000 ) ) ;
#7217 = FACE_OUTER_BOUND ( 'NONE', #3866, .T. ) ;
#7218 = CARTESIAN_POINT ( 'NONE',  ( 303.3333333333333144, -25.00000000000000000, -222.5000000000000853 ) ) ;
#7219 = ORIENTED_EDGE ( 'NONE', *, *, #10381, .F. ) ;
#7220 = CIRCLE ( 'NONE', #9077, 2.500000000000002220 ) ;
#7221 = CARTESIAN_POINT ( 'NONE',  ( -0.7826237921249277196, 0.000000000000000000, -11.05000000000000071 ) ) ;
#7222 = VECTOR ( 'NONE', #2309, 1000.000000000000000 ) ;
#7223 = AXIS2_PLACEMENT_3D ( 'NONE', #4342, #12166, #6659 ) ;
#7224 = DIRECTION ( 'NONE',  ( 2.312964634635743450E-16, 1.000000000000000000, 0.000000000000000000 ) ) ;
#7225 = DIRECTION ( 'NONE',  ( -1.000000000000000000, 0.000000000000000000, 0.000000000000000000 ) ) ;
#7226 = LINE ( 'NONE', #5210, #2782 ) ;
#7227 = AXIS2_PLACEMENT_3D ( 'NONE', #3153, #2040, #2188 ) ;
#7228 = CYLINDRICAL_SURFACE ( 'NONE', #8953, 5.000000000000004441 ) ;
#7229 = ORIENTED_EDGE ( 'NONE', *, *, #8875, .T. ) ;
#7230 = CARTESIAN_POINT ( 'NONE',  ( 140.0000000000000000, -95.00000000000008527, -169.9999999999999716 ) ) ;
#7231 = VECTOR ( 'NONE', #3464, 1000.000000000000000 ) ;
#7232 = EDGE_CURVE ( 'NONE', #2861, #6636, #3175, .T. ) ;
#7233 = DIRECTION ( 'NONE',  ( -1.000000000000000000, 0.000000000000000000, 0.000000000000000000 ) ) ;
#7234 = AXIS2_PLACEMENT_3D ( 'NONE', #1238, #10172, #12283 ) ;
#7235 = PRESENTATION_LAYER_ASSIGNMENT (  '', '', ( #5399 ) ) ;
#7236 = ORIENTED_EDGE ( 'NONE', *, *, #14113, .F. ) ;
#7237 = VECTOR ( 'NONE', #11460, 1000.000000000000000 ) ;
#7238 = DIRECTION ( 'NONE',  ( 0.000000000000000000, 0.000000000000000000, 1.000000000000000000 ) ) ;
#7239 = CARTESIAN_POINT ( 'NONE',  ( 1.800000000000001155, 0.000000000000000000, 0.000000000000000000 ) ) ;
#7240 =( REPRESENTATION_RELATIONSHIP ('NONE','NONE', #11251, #208 ) REPRESENTATION_RELATIONSHIP_WITH_TRANSFORMATION ( #1285 )SHAPE_REPRESENTATION_RELATIONSHIP( ) );
#7241 = CARTESIAN_POINT ( 'NONE',  ( -2.000000000000000888, 12.77500000000000036, 0.000000000000000000 ) ) ;
#7242 = DIRECTION ( 'NONE',  ( -0.000000000000000000, -0.000000000000000000, -1.000000000000000000 ) ) ;
#7243 = FACE_BOUND ( 'NONE', #12129, .T. ) ;
#7244 = VECTOR ( 'NONE', #4396, 1000.000000000000114 ) ;
#7245 = CARTESIAN_POINT ( 'NONE',  ( 4.000000000000000000, 2.309401076758515803, -0.4999999999999995559 ) ) ;
#7246 = CONTEXT_DEPENDENT_SHAPE_REPRESENTATION ( #12153, #10775 ) ;
#7247 = PRODUCT_DEFINITION_FORMATION_WITH_SPECIFIED_SOURCE ( 'ANY', '', #6922, .NOT_KNOWN. ) ;
#7248 = ORIENTED_EDGE ( 'NONE', *, *, #12694, .T. ) ;
#7249 = FACE_OUTER_BOUND ( 'NONE', #5374, .T. ) ;
#7250 = VERTEX_POINT ( 'NONE', #2910 ) ;
#7251 = CARTESIAN_POINT ( 'NONE',  ( 299.9999999999999432, -95.00000000000008527, -190.0000000000000000 ) ) ;
#7252 = CARTESIAN_POINT ( 'NONE',  ( 0.000000000000000000, 2.357898499370433054, -1.951563910473907981E-15 ) ) ;
#7253 = VERTEX_POINT ( 'NONE', #11971 ) ;
#7254 = CARTESIAN_POINT ( 'NONE',  ( -4.211140560182196957, 2.431303136016537803, -3.745885042887433514 ) ) ;
#7255 = EDGE_LOOP ( 'NONE', ( #4670, #5878, #12645, #2450 ) ) ;
#7256 = CARTESIAN_POINT ( 'NONE',  ( 170.9999999999999716, -8.660254037844389075, 200.0000000000000000 ) ) ;
#7257 = CARTESIAN_POINT ( 'NONE',  ( 140.0000000000000000, -95.00000000000008527, -186.2999999999999829 ) ) ;
#7258 = ORIENTED_EDGE ( 'NONE', *, *, #3677, .T. ) ;
#7259 = EDGE_CURVE ( 'NONE', #6389, #9136, #336, .T. ) ;
#7260 = CARTESIAN_POINT ( 'NONE',  ( 303.3333333333333144, -20.00000000000000000, -225.1500000000000625 ) ) ;
#7261 = SURFACE_STYLE_USAGE ( .BOTH. , #13928 ) ;
#7262 = SHAPE_DEFINITION_REPRESENTATION ( #8896, #11637 ) ;
#7263 = DIRECTION ( 'NONE',  ( 0.000000000000000000, 0.000000000000000000, 1.000000000000000000 ) ) ;
#7264 = EDGE_LOOP ( 'NONE', ( #3502, #8704, #12575 ) ) ;
#7265 = VERTEX_POINT ( 'NONE', #14134 ) ;
#7266 = DIRECTION ( 'NONE',  ( 0.000000000000000000, -1.000000000000000000, 0.000000000000000000 ) ) ;
#7267 = B_SPLINE_CURVE_WITH_KNOTS ( 'NONE', 3,
 ( #12693, #6969, #3845, #2763 ),
 .UNSPECIFIED., .F., .F.,
 ( 4, 4 ),
 ( 0.004656695506220394354, 0.007337072593346776264 ),
 .UNSPECIFIED. ) ;
#7268 = VERTEX_POINT ( 'NONE', #12990 ) ;
#7269 = CARTESIAN_POINT ( 'NONE',  ( 2.687328764639642653, -3.067272167851299969, -0.05923475698271395140 ) ) ;
#7270 = ORIENTED_EDGE ( 'NONE', *, *, #8842, .T. ) ;
#7271 = CARTESIAN_POINT ( 'NONE',  ( -124.9999999999999432, 55.00000000000001421, 40.00000000000000000 ) ) ;
#7272 = ORIENTED_EDGE ( 'NONE', *, *, #7868, .T. ) ;
#7273 = CARTESIAN_POINT ( 'NONE',  ( -145.0000000000000284, -75.00000000000008527, -14.14213562373090127 ) ) ;
#7274 = DIRECTION ( 'NONE',  ( -0.000000000000000000, -0.000000000000000000, 1.000000000000000000 ) ) ;
#7275 = PLANE ( 'NONE',  #2234 ) ;
#7276 = EDGE_CURVE ( 'NONE', #6389, #10563, #5169, .T. ) ;
#7277 = DIRECTION ( 'NONE',  ( -0.000000000000000000, -0.000000000000000000, -1.000000000000000000 ) ) ;
#7278 = CARTESIAN_POINT ( 'NONE',  ( 206.1500000000000057, -85.00000000000007105, 50.00000000000001421 ) ) ;
#7279 = DIRECTION ( 'NONE',  ( -1.000000000000000000, 0.000000000000000000, -0.000000000000000000 ) ) ;
#7280 = PRODUCT_DEFINITION_SHAPE ( 'NONE', 'NONE',  #14372 ) ;
#7281 = EDGE_LOOP ( 'NONE', ( #6244, #7555 ) ) ;
#7282 = ORIENTED_EDGE ( 'NONE', *, *, #878, .F. ) ;
#7283 = EDGE_CURVE ( 'NONE', #8115, #663, #4775, .T. ) ;
#7284 = EDGE_CURVE ( 'NONE', #11114, #13361, #1811, .T. ) ;
#7285 = DIRECTION ( 'NONE',  ( 1.000000000000000000, 0.000000000000000000, 0.000000000000000000 ) ) ;
#7286 = ADVANCED_FACE ( 'NONE', ( #8480 ), #8700, .T. ) ;
#7287 = VERTEX_POINT ( 'NONE', #7606 ) ;
#7288 = DIRECTION ( 'NONE',  ( -0.000000000000000000, -0.000000000000000000, 1.000000000000000000 ) ) ;
#7289 = CARTESIAN_POINT ( 'NONE',  ( 219.9999999999999716, -14.99999999999999822, 222.5000000000000853 ) ) ;
#7290 = FACE_BOUND ( 'NONE', #11732, .T. ) ;
#7291 = VERTEX_POINT ( 'NONE', #7400 ) ;
#7292 = CARTESIAN_POINT ( 'NONE',  ( 0.000000000000000000, 0.000000000000000000, -200.0000000000000000 ) ) ;
#7293 = DIRECTION ( 'NONE',  ( 0.000000000000000000, 0.000000000000000000, 1.000000000000000000 ) ) ;
#7294 = CARTESIAN_POINT ( 'NONE',  ( 439.9999999999999432, -20.00000000000000355, -169.9999999999999716 ) ) ;
#7295 = LINE ( 'NONE', #7369, #13660 ) ;
#7296 = APPLICATION_CONTEXT ( 'automotive_design' ) ;
#7297 = CIRCLE ( 'NONE', #788, 2.649999999999985700 ) ;
#7298 = ORIENTED_EDGE ( 'NONE', *, *, #9072, .F. ) ;
#7299 = DIRECTION ( 'NONE',  ( -2.312964634635743450E-16, -1.000000000000000000, 0.000000000000000000 ) ) ;
#7300 = ADVANCED_FACE ( 'NONE', ( #6312 ), #11829, .T. ) ;
#7301 = CARTESIAN_POINT ( 'NONE',  ( 124.9999999999999574, -64.99999999999997158, 10.00000000000000000 ) ) ;
#7302 = VERTEX_POINT ( 'NONE', #13399 ) ;
#7303 = DIRECTION ( 'NONE',  ( 0.000000000000000000, -1.000000000000000000, 0.000000000000000000 ) ) ;
#7304 = EDGE_CURVE ( 'NONE', #11887, #9938, #1211, .T. ) ;
#7305 = CIRCLE ( 'NONE', #13095, 5.000000000000004441 ) ;
#7306 = CARTESIAN_POINT ( 'NONE',  ( 201.0000000000000000, -85.00000000000007105, 190.0000000000000000 ) ) ;
#7307 = CIRCLE ( 'NONE', #324, 11.05000000000000071 ) ;
#7308 = DIRECTION ( 'NONE',  ( 0.000000000000000000, 0.000000000000000000, 1.000000000000000000 ) ) ;
#7309 = LINE ( 'NONE', #3910, #10871 ) ;
#7310 = CARTESIAN_POINT ( 'NONE',  ( -1.360585162435467455, 4.061296242128285883, -3.505054077164959203 ) ) ;
#7311 = EDGE_LOOP ( 'NONE', ( #1203, #10944, #5188, #7515 ) ) ;
#7312 = CARTESIAN_POINT ( 'NONE',  ( 302.6499999999999204, -75.00000000000008527, -186.2999999999999829 ) ) ;
#7313 = AXIS2_PLACEMENT_3D ( 'NONE', #10215, #1277, #3415 ) ;
#7314 = ORIENTED_EDGE ( 'NONE', *, *, #7513, .T. ) ;
#7315 = CARTESIAN_POINT ( 'NONE',  ( 1.800000000000002931, 0.000000000000000000, 0.000000000000000000 ) ) ;
#7316 = CARTESIAN_POINT ( 'NONE',  ( -297.4999999999999432, -75.00000000000008527, 339.9999999999999432 ) ) ;
#7317 = ADVANCED_BREP_SHAPE_REPRESENTATION ( '', ( #8329, #14039 ), #11646 ) ;
#7318 = VECTOR ( 'NONE', #12602, 1000.000000000000000 ) ;
#7319 = EDGE_LOOP ( 'NONE', ( #7418, #11344, #12553, #11537 ) ) ;
#7320 = CARTESIAN_POINT ( 'NONE',  ( 132.4999999999999432, -36.99999999999997868, -169.9999999999999716 ) ) ;
#7321 = VERTEX_POINT ( 'NONE', #3351 ) ;
#7322 = DIRECTION ( 'NONE',  ( -1.000000000000000000, 0.000000000000000000, 0.000000000000000000 ) ) ;
#7323 = FACE_OUTER_BOUND ( 'NONE', #12449, .T. ) ;
#7324 = VERTEX_POINT ( 'NONE', #5789 ) ;
#7325 = CIRCLE ( 'NONE', #11974, 2.055000000000001492 ) ;
#7326 = FILL_AREA_STYLE ('',( #2913 ) ) ;
#7327 = PLANE ( 'NONE',  #7406 ) ;
#7328 = AXIS2_PLACEMENT_3D ( 'NONE', #4488, #12504, #6584 ) ;
#7329 = EDGE_CURVE ( 'NONE', #1810, #417, #7777, .T. ) ;
#7330 = CONTEXT_DEPENDENT_SHAPE_REPRESENTATION ( #9937, #406 ) ;
#7331 = VECTOR ( 'NONE', #8442, 1000.000000000000000 ) ;
#7332 = PLANE ( 'NONE',  #10133 ) ;
#7333 = VERTEX_POINT ( 'NONE', #5650 ) ;
#7334 = VERTEX_POINT ( 'NONE', #13269 ) ;
#7335 = CARTESIAN_POINT ( 'NONE',  ( 360.0000000000000000, 55.00000000000001421, 0.000000000000000000 ) ) ;
#7336 = CONICAL_SURFACE ( 'NONE', #3873, 2.041999999999999815, 1.047197551196591858 ) ;
#7337 = ORIENTED_EDGE ( 'NONE', *, *, #5967, .T. ) ;
#7338 = DIRECTION ( 'NONE',  ( 0.000000000000000000, 0.000000000000000000, 1.000000000000000000 ) ) ;
#7339 = CIRCLE ( 'NONE', #1066, 2.649999999999985700 ) ;
#7340 = ORIENTED_EDGE ( 'NONE', *, *, #8607, .F. ) ;
#7341 = PLANE ( 'NONE',  #6871 ) ;
#7342 = VERTEX_POINT ( 'NONE', #3276 ) ;
#7343 = FACE_BOUND ( 'NONE', #477, .T. ) ;
#7344 = AXIS2_PLACEMENT_3D ( 'NONE', #14226, #10032, #56 ) ;
#7345 = VECTOR ( 'NONE', #13707, 1000.000000000000000 ) ;
#7346 = CARTESIAN_POINT ( 'NONE',  ( 53.33333333333330017, -25.00000000000000000, 225.1500000000000625 ) ) ;
#7347 = CARTESIAN_POINT ( 'NONE',  ( 2.500000000000000000, -1.178949249685218748, -2.041999999999998039 ) ) ;
#7348 = CIRCLE ( 'NONE', #8743, 4.000000000000000000 ) ;
#7349 = LINE ( 'NONE', #5189, #12316 ) ;
#7350 = LINE ( 'NONE', #8433, #3729 ) ;
#7351 = AXIS2_PLACEMENT_3D ( 'NONE', #778, #13061, #12116 ) ;
#7352 = DIRECTION ( 'NONE',  ( -0.000000000000000000, -0.000000000000000000, -1.000000000000000000 ) ) ;
#7353 = ORIENTED_EDGE ( 'NONE', *, *, #5607, .T. ) ;
#7354 = VECTOR ( 'NONE', #8004, 1000.000000000000000 ) ;
#7355 = ORIENTED_EDGE ( 'NONE', *, *, #6668, .T. ) ;
#7356 = CIRCLE ( 'NONE', #10610, 4.250000000000000000 ) ;
#7357 = EDGE_CURVE ( 'NONE', #11325, #5316, #5255, .T. ) ;
#7358 = DIRECTION ( 'NONE',  ( 1.000000000000000000, 0.000000000000000000, 0.000000000000000000 ) ) ;
#7359 = EDGE_CURVE ( 'NONE', #13709, #13005, #9053, .T. ) ;
#7360 = CARTESIAN_POINT ( 'NONE',  ( 239.1499999999999204, -85.00000000000007105, 55.00000000000001421 ) ) ;
#7361 = CARTESIAN_POINT ( 'NONE',  ( -5.384454397937118664, 6.702023979852544604E-16, -5.000000000000000000 ) ) ;
#7362 = CARTESIAN_POINT ( 'NONE',  ( 357.0000000000000000, -8.660254037844389075, 199.9990000000000236 ) ) ;
#7363 = EDGE_LOOP ( 'NONE', ( #10665, #699, #13887, #3842 ) ) ;
#7364 = CIRCLE ( 'NONE', #1097, 20.00000000000000000 ) ;
#7365 = DIRECTION ( 'NONE',  ( 0.000000000000000000, 0.000000000000000000, -1.000000000000000000 ) ) ;
#7366 = EDGE_CURVE ( 'NONE', #7265, #5572, #2452, .T. ) ;
#7367 = CARTESIAN_POINT ( 'NONE',  ( 0.000000000000000000, 0.000000000000000000, -200.0000000000000000 ) ) ;
#7368 = DIRECTION ( 'NONE',  ( 1.000000000000000000, 0.000000000000000000, 0.000000000000000000 ) ) ;
#7369 = CARTESIAN_POINT ( 'NONE',  ( 197.5000000000000000, -80.00000000000007105, 55.00000000000001421 ) ) ;
#7370 = CIRCLE ( 'NONE', #12938, 2.649999999999985700 ) ;
#7371 = EDGE_LOOP ( 'NONE', ( #11026, #13611, #6670, #10101 ) ) ;
#7372 = VERTEX_POINT ( 'NONE', #9940 ) ;
#7373 = EDGE_CURVE ( 'NONE', #14164, #12252, #12187, .T. ) ;
#7374 = CARTESIAN_POINT ( 'NONE',  ( 2.500000000000000000, 0.000000000000000000, 0.000000000000000000 ) ) ;
#7375 = AXIS2_PLACEMENT_3D ( 'NONE', #4756, #7930, #5761 ) ;
#7376 = DIRECTION ( 'NONE',  ( 1.000000000000000000, 0.000000000000000000, 0.000000000000000000 ) ) ;
#7377 = ORIENTED_EDGE ( 'NONE', *, *, #3174, .T. ) ;
#7378 = DIRECTION ( 'NONE',  ( -1.000000000000000000, 0.000000000000000000, 0.000000000000000000 ) ) ;
#7379 = SHAPE_REPRESENTATION_RELATIONSHIP ( 'NONE' , 'NONE' ,  #5332, #13210 ) ;
#7380 = DIRECTION ( 'NONE',  ( 0.000000000000000000, 0.000000000000000000, -1.000000000000000000 ) ) ;
#7381 = ADVANCED_FACE ( 'NONE', ( #2240 ), #6875, .F. ) ;
#7382 = EDGE_CURVE ( 'NONE', #13697, #11046, #113, .T. ) ;
#7383 = LINE ( 'NONE', #13906, #3503 ) ;
#7384 = LINE ( 'NONE', #9495, #13179 ) ;
#7385 = SURFACE_STYLE_USAGE ( .BOTH. , #8618 ) ;
#7386 = ADVANCED_FACE ( 'NONE', ( #13469, #3551 ), #11027, .T. ) ;
#7387 = EDGE_CURVE ( 'NONE', #1338, #3461, #8847, .T. ) ;
#7388 = CIRCLE ( 'NONE', #7847, 4.000000000000000000 ) ;
#7389 = ITEM_DEFINED_TRANSFORMATION ( 'NONE', 'NONE', #11873,  #14039 ) ;
#7390 = EDGE_LOOP ( 'NONE', ( #8455, #12832 ) ) ;
#7391 = ADVANCED_FACE ( 'NONE', ( #6809 ), #2387, .F. ) ;
#7392 = DIRECTION ( 'NONE',  ( 0.000000000000000000, 0.000000000000000000, -1.000000000000000000 ) ) ;
#7393 = VERTEX_POINT ( 'NONE', #4500 ) ;
#7394 = CARTESIAN_POINT ( 'NONE',  ( 1.567478505476134606E-15, 4.618802153517012066, -3.433295621305382905 ) ) ;
#7395 = DIRECTION ( 'NONE',  ( 1.000000000000000000, 0.000000000000000000, 0.000000000000000000 ) ) ;
#7396 = ORIENTED_EDGE ( 'NONE', *, *, #5081, .F. ) ;
#7397 = LINE ( 'NONE', #6385, #3879 ) ;
#7398 = VERTEX_POINT ( 'NONE', #1353 ) ;
#7399 = CIRCLE ( 'NONE', #11572, 5.000000000000004441 ) ;
#7400 = CARTESIAN_POINT ( 'NONE',  ( 136.6666666666666288, -20.00000000000000000, -225.1500000000000625 ) ) ;
#7401 = PRODUCT_DEFINITION_SHAPE ( 'NONE', 'NONE',  #14371 ) ;
#7402 = DIRECTION ( 'NONE',  ( 1.000000000000000000, 0.000000000000000000, 0.000000000000000000 ) ) ;
#7403 = ORIENTED_EDGE ( 'NONE', *, *, #11535, .T. ) ;
#7404 = CARTESIAN_POINT ( 'NONE',  ( 119.9999999999999147, -225.0010000000000048, -19.99999999999998934 ) ) ;
#7405 = CIRCLE ( 'NONE', #1124, 12.00000000000000000 ) ;
#7406 = AXIS2_PLACEMENT_3D ( 'NONE', #7478, #9517, #6104 ) ;
#7407 = FACE_OUTER_BOUND ( 'NONE', #2168, .T. ) ;
#7408 = SURFACE_STYLE_FILL_AREA ( #5379 ) ;
#7409 = CARTESIAN_POINT ( 'NONE',  ( 119.9999999999999147, -20.00000000000000000, 169.9999999999999716 ) ) ;
#7410 = CARTESIAN_POINT ( 'NONE',  ( 53.33333333333330017, -25.00000000000000000, 222.5000000000000853 ) ) ;
#7411 = ORIENTED_EDGE ( 'NONE', *, *, #603, .T. ) ;
#7412 = ORIENTED_EDGE ( 'NONE', *, *, #705, .T. ) ;
#7413 = FACE_BOUND ( 'NONE', #638, .T. ) ;
#7414 = EDGE_LOOP ( 'NONE', ( #12765, #10276, #8170, #9381 ) ) ;
#7415 = TOROIDAL_SURFACE ( 'NONE', #1136, 4.000000000000000000, 0.2500000000000000000 ) ;
#7416 = VECTOR ( 'NONE', #6383, 1000.000000000000000 ) ;
#7417 = DIRECTION ( 'NONE',  ( -0.000000000000000000, 1.000000000000000000, -0.000000000000000000 ) ) ;
#7418 = ORIENTED_EDGE ( 'NONE', *, *, #2300, .F. ) ;
#7419 =( GEOMETRIC_REPRESENTATION_CONTEXT ( 3 ) GLOBAL_UNCERTAINTY_ASSIGNED_CONTEXT ( ( #4161 ) ) GLOBAL_UNIT_ASSIGNED_CONTEXT ( ( #7540, #4222, #14075 ) ) REPRESENTATION_CONTEXT ( 'NONE', 'WORKASPACE' ) );
#7420 = EDGE_CURVE ( 'NONE', #12064, #2437, #7557, .T. ) ;
#7421 = ORIENTED_EDGE ( 'NONE', *, *, #1636, .F. ) ;
#7422 = DIRECTION ( 'NONE',  ( 1.000000000000000000, 0.000000000000000000, -0.000000000000000000 ) ) ;
#7423 = ORIENTED_EDGE ( 'NONE', *, *, #13053, .F. ) ;
#7424 = DIRECTION ( 'NONE',  ( 1.000000000000000000, 0.000000000000000000, 0.000000000000000000 ) ) ;
#7425 = LINE ( 'NONE', #2865, #5959 ) ;
#7426 = LINE ( 'NONE', #6556, #11293 ) ;
#7427 = VECTOR ( 'NONE', #7193, 1000.000000000000000 ) ;
#7428 = PLANE ( 'NONE',  #8539 ) ;
#7429 = VERTEX_POINT ( 'NONE', #6740 ) ;
#7430 = AXIS2_PLACEMENT_3D ( 'NONE', #10222, #11449, #1567 ) ;
#7431 = ORIENTED_EDGE ( 'NONE', *, *, #11462, .T. ) ;
#7432 = CARTESIAN_POINT ( 'NONE',  ( 294.4999999999999432, -95.00000000000008527, -190.0000000000000000 ) ) ;
#7433 = ADVANCED_FACE ( 'NONE', ( #8985 ), #10072, .F. ) ;
#7434 = VECTOR ( 'NONE', #6059, 1000.000000000000000 ) ;
#7435 = ORIENTED_EDGE ( 'NONE', *, *, #517, .T. ) ;
#7436 = CARTESIAN_POINT ( 'NONE',  ( 197.5000000000000000, -80.00000000000007105, 50.00000000000001421 ) ) ;
#7437 = DIRECTION ( 'NONE',  ( 1.000000000000000000, 0.000000000000000000, -0.000000000000000000 ) ) ;
#7438 = FACE_BOUND ( 'NONE', #7464, .T. ) ;
#7439 = ORIENTED_EDGE ( 'NONE', *, *, #9534, .T. ) ;
#7440 = CIRCLE ( 'NONE', #7885, 0.8509999999999999787 ) ;
#7441 = DIRECTION ( 'NONE',  ( 0.000000000000000000, -0.000000000000000000, 1.000000000000000000 ) ) ;
#7442 = EDGE_CURVE ( 'NONE', #1365, #13895, #13331, .T. ) ;
#7443 = DIRECTION ( 'NONE',  ( -0.000000000000000000, -0.000000000000000000, -1.000000000000000000 ) ) ;
#7444 = DIRECTION ( 'NONE',  ( 0.000000000000000000, 0.000000000000000000, -1.000000000000000000 ) ) ;
#7445 = AXIS2_PLACEMENT_3D ( 'NONE', #2209, #6638, #3522 ) ;
#7446 = DIRECTION ( 'NONE',  ( -1.000000000000000000, -0.000000000000000000, -0.000000000000000000 ) ) ;
#7447 = ORIENTED_EDGE ( 'NONE', *, *, #4743, .T. ) ;
#7448 =( GEOMETRIC_REPRESENTATION_CONTEXT ( 3 ) GLOBAL_UNCERTAINTY_ASSIGNED_CONTEXT ( ( #4359 ) ) GLOBAL_UNIT_ASSIGNED_CONTEXT ( ( #7754, #13477, #12055 ) ) REPRESENTATION_CONTEXT ( 'NONE', 'WORKASPACE' ) );
#7449 = EDGE_LOOP ( 'NONE', ( #2118, #4813, #7501, #3612, #7036 ) ) ;
#7450 = DIRECTION ( 'NONE',  ( 1.000000000000000000, 0.000000000000000000, 0.000000000000000000 ) ) ;
#7451 = DIRECTION ( 'NONE',  ( 0.000000000000000000, 1.000000000000000000, -1.287488025362403787E-15 ) ) ;
#7452 = AXIS2_PLACEMENT_3D ( 'NONE', #3590, #7992, #12434 ) ;
#7453 = ORIENTED_EDGE ( 'NONE', *, *, #11718, .F. ) ;
#7454 = LINE ( 'NONE', #14192, #12657 ) ;
#7455 = DIRECTION ( 'NONE',  ( -0.000000000000000000, -0.000000000000000000, -1.000000000000000000 ) ) ;
#7456 = EDGE_CURVE ( 'NONE', #10523, #11569, #7814, .T. ) ;
#7457 = DIRECTION ( 'NONE',  ( -0.000000000000000000, 1.000000000000000000, -0.000000000000000000 ) ) ;
#7458 = DIRECTION ( 'NONE',  ( 1.000000000000000000, 0.000000000000000000, 0.000000000000000000 ) ) ;
#7459 = VECTOR ( 'NONE', #4399, 1000.000000000000000 ) ;
#7460 = ORIENTED_EDGE ( 'NONE', *, *, #14290, .T. ) ;
#7461 = DIRECTION ( 'NONE',  ( 1.000000000000000000, 0.000000000000000000, 0.000000000000000000 ) ) ;
#7462 = AXIS2_PLACEMENT_3D ( 'NONE', #12738, #8602, #1856 ) ;
#7463 = STYLED_ITEM ( 'NONE', ( #4454 ), #12845 ) ;
#7464 = EDGE_LOOP ( 'NONE', ( #11606, #211 ) ) ;
#7465 = VECTOR ( 'NONE', #11923, 1000.000000000000000 ) ;
#7466 = FACE_OUTER_BOUND ( 'NONE', #14153, .T. ) ;
#7467 = DIRECTION ( 'NONE',  ( -0.000000000000000000, -0.000000000000000000, -1.000000000000000000 ) ) ;
#7468 = EDGE_CURVE ( 'NONE', #7879, #8555, #4927, .T. ) ;
#7469 = EDGE_CURVE ( 'NONE', #2766, #11206, #4548, .T. ) ;
#7470 = EDGE_LOOP ( 'NONE', ( #2291, #3518, #912, #1230 ) ) ;
#7471 = ADVANCED_FACE ( 'NONE', ( #6149 ), #1751, .T. ) ;
#7472 = DIRECTION ( 'NONE',  ( 1.000000000000000000, 0.000000000000000000, 0.000000000000000000 ) ) ;
#7473 = ORIENTED_EDGE ( 'NONE', *, *, #4191, .T. ) ;
#7474 = CARTESIAN_POINT ( 'NONE',  ( 259.0000000000000000, -8.660254037844389075, 199.9990000000000236 ) ) ;
#7475 = DIRECTION ( 'NONE',  ( 0.000000000000000000, 0.000000000000000000, 1.000000000000000000 ) ) ;
#7477 = ORIENTED_EDGE ( 'NONE', *, *, #968, .T. ) ;
#7476 = CIRCLE ( 'NONE', #2155, 1.037871761867652065 ) ;
#7478 = CARTESIAN_POINT ( 'NONE',  ( 2.500000000000000000, 2.357898499370433054, -1.951563910473907981E-15 ) ) ;
#7479 = ORIENTED_EDGE ( 'NONE', *, *, #3733, .T. ) ;
#7480 = STYLED_ITEM ( 'NONE', ( #6321 ), #13031 ) ;
#7481 = CARTESIAN_POINT ( 'NONE',  ( 79.99999999999971578, 35.00000000000000000, 10.00000000000000000 ) ) ;
#7482 = ITEM_DEFINED_TRANSFORMATION ( 'NONE', 'NONE', #729,  #14039 ) ;
#7483 = DIRECTION ( 'NONE',  ( -0.000000000000000000, 0.000000000000000000, -1.000000000000000000 ) ) ;
#7484 = EDGE_LOOP ( 'NONE', ( #4232, #13643 ) ) ;
#7485 = ORIENTED_EDGE ( 'NONE', *, *, #613, .F. ) ;
#7486 = CARTESIAN_POINT ( 'NONE',  ( 219.9999999999999716, -85.00000000000007105, 170.0000000000000000 ) ) ;
#7487 = AXIS2_PLACEMENT_3D ( 'NONE', #12110, #2169, #10668 ) ;
#7488 = ORIENTED_EDGE ( 'NONE', *, *, #4171, .T. ) ;
#7489 = CARTESIAN_POINT ( 'NONE',  ( -314.9999999999999432, 55.00000000000001421, 40.00000000000000000 ) ) ;
#7490 = EDGE_LOOP ( 'NONE', ( #857, #11543, #7532, #5783 ) ) ;
#7491 = ORIENTED_EDGE ( 'NONE', *, *, #7284, .F. ) ;
#7492 = CARTESIAN_POINT ( 'NONE',  ( 386.6666666666666288, -20.00000000000000000, 222.5000000000000853 ) ) ;
#7493 = EDGE_LOOP ( 'NONE', ( #3718, #10640 ) ) ;
#7494 = DIRECTION ( 'NONE',  ( 1.000000000000000000, 0.000000000000000000, 0.000000000000000000 ) ) ;
#7495 = DIRECTION ( 'NONE',  ( 0.000000000000000000, 0.000000000000000000, 1.000000000000000000 ) ) ;
#7496 = PLANE ( 'NONE',  #5953 ) ;
#7497 = CARTESIAN_POINT ( 'NONE',  ( 2.740000000000000213, 0.000000000000000000, 0.000000000000000000 ) ) ;
#7498 = CARTESIAN_POINT ( 'NONE',  ( 269.0000000000000000, -8.660254037844389075, 205.0000000000000284 ) ) ;
#7499 = ORIENTED_EDGE ( 'NONE', *, *, #10908, .T. ) ;
#7500 = ADVANCED_FACE ( 'NONE', ( #9197 ), #4996, .F. ) ;
#7501 = ORIENTED_EDGE ( 'NONE', *, *, #2723, .F. ) ;
#7502 = CARTESIAN_POINT ( 'NONE',  ( -299.9999999999999432, -75.00000000000008527, 329.9999999999999432 ) ) ;
#7503 = AXIS2_PLACEMENT_3D ( 'NONE', #8780, #9945, #12181 ) ;
#7504 = EDGE_LOOP ( 'NONE', ( #13418, #2539, #880, #4043 ) ) ;
#7505 = CARTESIAN_POINT ( 'NONE',  ( -299.9999999999999432, -75.00000000000008527, 339.9999999999999432 ) ) ;
#7506 = CARTESIAN_POINT ( 'NONE',  ( 3.900000000000000799, 0.000000000000000000, 0.000000000000000000 ) ) ;
#7507 = LINE ( 'NONE', #2067, #380 ) ;
#7508 = ORIENTED_EDGE ( 'NONE', *, *, #16, .F. ) ;
#7509 = DIRECTION ( 'NONE',  ( 0.000000000000000000, -1.287488025362403787E-15, -1.000000000000000000 ) ) ;
#7510 = CARTESIAN_POINT ( 'NONE',  ( 303.3333333333333144, -20.00000000000000000, -222.5000000000000853 ) ) ;
#7511 = DIRECTION ( 'NONE',  ( 6.123233995736766036E-17, 0.000000000000000000, 1.000000000000000000 ) ) ;
#7512 = DIRECTION ( 'NONE',  ( 0.000000000000000000, 0.000000000000000000, -1.000000000000000000 ) ) ;
#7513 = EDGE_CURVE ( 'NONE', #10689, #5572, #6860, .T. ) ;
#7514 = VERTEX_POINT ( 'NONE', #10578 ) ;
#7515 = ORIENTED_EDGE ( 'NONE', *, *, #6688, .F. ) ;
#7516 = FACE_BOUND ( 'NONE', #1802, .T. ) ;
#7517 = AXIS2_PLACEMENT_3D ( 'NONE', #3146, #5451, #6399 ) ;
#7518 = PLANE ( 'NONE',  #11842 ) ;
#7519 = EDGE_CURVE ( 'NONE', #2281, #11600, #12647, .T. ) ;
#7520 = ORIENTED_EDGE ( 'NONE', *, *, #2883, .T. ) ;
#7521 = DIRECTION ( 'NONE',  ( -0.000000000000000000, 1.000000000000000000, -0.000000000000000000 ) ) ;
#7522 = CARTESIAN_POINT ( 'NONE',  ( 1.794155980045909482, 0.000000000000000000, 4.300000000000001599 ) ) ;
#7523 = DIRECTION ( 'NONE',  ( -1.000000000000000000, 0.000000000000000000, 0.000000000000000000 ) ) ;
#7524 = AXIS2_PLACEMENT_3D ( 'NONE', #1542, #10056, #79 ) ;
#7525 = ORIENTED_EDGE ( 'NONE', *, *, #11156, .T. ) ;
#7526 = CARTESIAN_POINT ( 'NONE',  ( 134.9999999999999716, 45.00000000000001421, 0.000000000000000000 ) ) ;
#7527 = ORIENTED_EDGE ( 'NONE', *, *, #5920, .T. ) ;
#7528 = DIRECTION ( 'NONE',  ( -1.000000000000000000, 0.000000000000000000, 0.000000000000000000 ) ) ;
#7529 = CARTESIAN_POINT ( 'NONE',  ( -5.000000000000000888, 8.660254037844390851, 210.0000000000000000 ) ) ;
#7530 = EDGE_CURVE ( 'NONE', #10602, #258, #6947, .T. ) ;
#7531 = ADVANCED_FACE ( 'NONE', ( #13613, #1714, #9126, #7083, #1563, #13828 ), #13532, .F. ) ;
#7532 = ORIENTED_EDGE ( 'NONE', *, *, #9415, .T. ) ;
#7533 = ORIENTED_EDGE ( 'NONE', *, *, #4469, .T. ) ;
#7534 = CARTESIAN_POINT ( 'NONE',  ( 132.3499999999999943, 45.00000000000001421, 10.00000000000000000 ) ) ;
#7535 = CARTESIAN_POINT ( 'NONE',  ( 2.100000000000000089, 0.000000000000000000, -5.000000000000000000 ) ) ;
#7536 = EDGE_LOOP ( 'NONE', ( #13213, #14184, #3534, #8588, #12075 ) ) ;
#7537 = DIRECTION ( 'NONE',  ( -0.000000000000000000, -0.000000000000000000, 1.000000000000000000 ) ) ;
#7538 = FACE_BOUND ( 'NONE', #1422, .T. ) ;
#7539 =( LENGTH_UNIT ( ) NAMED_UNIT ( * ) SI_UNIT ( .MILLI., .METRE. ) );
#7540 =( LENGTH_UNIT ( ) NAMED_UNIT ( * ) SI_UNIT ( .MILLI., .METRE. ) );
#7541 = ADVANCED_FACE ( 'NONE', ( #2530 ), #11378, .F. ) ;
#7542 = CARTESIAN_POINT ( 'NONE',  ( -4.000000000000000000, -0.8232339106130515116, -3.430630286862743183 ) ) ;
#7543 = AXIS2_PLACEMENT_3D ( 'NONE', #9887, #3084, #7424 ) ;
#7544 = ORIENTED_EDGE ( 'NONE', *, *, #4456, .F. ) ;
#7545 = ORIENTED_EDGE ( 'NONE', *, *, #4605, .T. ) ;
#7546 = CARTESIAN_POINT ( 'NONE',  ( 13.50000000000000000, 0.000000000000000000, 190.0000000000000000 ) ) ;
#7547 = EDGE_LOOP ( 'NONE', ( #12198, #9882, #7775, #4190 ) ) ;
#7548 = DIRECTION ( 'NONE',  ( -0.000000000000000000, -1.000000000000000000, -0.000000000000000000 ) ) ;
#7549 = EDGE_CURVE ( 'NONE', #7398, #4493, #8171, .T. ) ;
#7550 = UNCERTAINTY_MEASURE_WITH_UNIT (LENGTH_MEASURE( 1.000000000000000082E-05 ), #9395, 'distance_accuracy_value', 'NONE');
#7551 = ORIENTED_EDGE ( 'NONE', *, *, #7790, .F. ) ;
#7552 = AXIS2_PLACEMENT_3D ( 'NONE', #7683, #12183, #4436 ) ;
#7553 = ORIENTED_EDGE ( 'NONE', *, *, #4832, .F. ) ;
#7554 = DIRECTION ( 'NONE',  ( -0.000000000000000000, -0.000000000000000000, -1.000000000000000000 ) ) ;
#7555 = ORIENTED_EDGE ( 'NONE', *, *, #5797, .T. ) ;
#7556 = CARTESIAN_POINT ( 'NONE',  ( 2.740000000000000213, -0.6774776749089226335, -0.5150000000000000133 ) ) ;
#7557 = CIRCLE ( 'NONE', #10331, 13.50000000000000000 ) ;
#7558 = DIRECTION ( 'NONE',  ( 1.000000000000000000, 0.000000000000000000, -0.000000000000000000 ) ) ;
#7559 = DIRECTION ( 'NONE',  ( 0.000000000000000000, -0.000000000000000000, -1.000000000000000000 ) ) ;
#7560 = VECTOR ( 'NONE', #9471, 1000.000000000000000 ) ;
#7561 = CARTESIAN_POINT ( 'NONE',  ( 0.000000000000000000, 0.000000000000000000, 0.000000000000000000 ) ) ;
#7562 = EDGE_CURVE ( 'NONE', #1151, #4587, #12672, .T. ) ;
#7563 = DIRECTION ( 'NONE',  ( 1.000000000000000000, 0.000000000000000000, 0.000000000000000000 ) ) ;
#7564 = CONICAL_SURFACE ( 'NONE', #10336, 2.500000000000002220, 1.029744260000002631 ) ;
#7565 = EDGE_LOOP ( 'NONE', ( #7403, #11254, #1477, #4014 ) ) ;
#7566 = EDGE_CURVE ( 'NONE', #1448, #12847, #11665, .T. ) ;
#7567 = AXIS2_PLACEMENT_3D ( 'NONE', #4622, #162, #2374 ) ;
#7568 = EDGE_LOOP ( 'NONE', ( #9929, #3649 ) ) ;
#7569 = AXIS2_PLACEMENT_3D ( 'NONE', #6991, #6724, #11153 ) ;
#7570 = EDGE_CURVE ( 'NONE', #4821, #7268, #8319, .T. ) ;
#7572 = CARTESIAN_POINT ( 'NONE',  ( 302.6499999999999204, -75.00000000000008527, -186.2999999999999829 ) ) ;
#7571 = AXIS2_PLACEMENT_3D ( 'NONE', #9531, #11852, #12791 ) ;
#7573 = ORIENTED_EDGE ( 'NONE', *, *, #13026, .T. ) ;
#7574 = CARTESIAN_POINT ( 'NONE',  ( 0.000000000000000000, 0.000000000000000000, -4.000000000000000000 ) ) ;
#7575 = LINE ( 'NONE', #12014, #4706 ) ;
#7576 = DIRECTION ( 'NONE',  ( -0.000000000000000000, 0.000000000000000000, 1.000000000000000000 ) ) ;
#7577 = VECTOR ( 'NONE', #1831, 1000.000000000000000 ) ;
#7578 = APPLICATION_CONTEXT ( 'automotive_design' ) ;
#7579 = ORIENTED_EDGE ( 'NONE', *, *, #4898, .T. ) ;
#7580 = AXIS2_PLACEMENT_3D ( 'NONE', #11404, #4591, #11333 ) ;
#7581 = DIRECTION ( 'NONE',  ( -1.000000000000000000, 0.000000000000000000, 0.000000000000000000 ) ) ;
#7582 = VECTOR ( 'NONE', #2652, 1000.000000000000114 ) ;
#7583 = CARTESIAN_POINT ( 'NONE',  ( 134.9999999999999432, -36.99999999999997868, -180.0000000000000000 ) ) ;
#7584 = DIRECTION ( 'NONE',  ( 6.123233995736766036E-17, 0.000000000000000000, -1.000000000000000000 ) ) ;
#7585 = AXIS2_PLACEMENT_3D ( 'NONE', #5537, #3439, #12277 ) ;
#7586 = FACE_OUTER_BOUND ( 'NONE', #3171, .T. ) ;
#7587 = ORIENTED_EDGE ( 'NONE', *, *, #443, .T. ) ;
#7588 = CONICAL_SURFACE ( 'NONE', #3647, 5.560781378645573980, 1.221730476396046816 ) ;
#7589 = VERTEX_POINT ( 'NONE', #12746 ) ;
#7590 = DIRECTION ( 'NONE',  ( -1.000000000000000000, -0.000000000000000000, -0.000000000000000000 ) ) ;
#7591 = VECTOR ( 'NONE', #10455, 1000.000000000000000 ) ;
#7592 = CARTESIAN_POINT ( 'NONE',  ( -5.000000000000000888, 8.660254037844390851, 200.0000000000000000 ) ) ;
#7593 = EDGE_CURVE ( 'NONE', #1872, #12690, #11280, .T. ) ;
#7594 = ORIENTED_EDGE ( 'NONE', *, *, #2229, .F. ) ;
#7595 = CARTESIAN_POINT ( 'NONE',  ( 0.2500000000000002220, 0.000000000000000000, 4.250000000000000000 ) ) ;
#7596 = DIRECTION ( 'NONE',  ( 6.123233995736766036E-17, -1.000000000000000000, 0.000000000000000000 ) ) ;
#7597 = CIRCLE ( 'NONE', #11193, 2.649999999999985700 ) ;
#7598 = ORIENTED_EDGE ( 'NONE', *, *, #11702, .T. ) ;
#7599 = CARTESIAN_POINT ( 'NONE',  ( 233.8499999999999375, -85.00000000000007105, 50.00000000000001421 ) ) ;
#7600 = VERTEX_POINT ( 'NONE', #12599 ) ;
#7601 = LINE ( 'NONE', #4209, #11628 ) ;
#7602 = PLANE ( 'NONE',  #9266 ) ;
#7603 = ADVANCED_FACE ( 'NONE', ( #10283 ), #13757, .F. ) ;
#7604 = ORIENTED_EDGE ( 'NONE', *, *, #4375, .F. ) ;
#7605 = ORIENTED_EDGE ( 'NONE', *, *, #3477, .T. ) ;
#7606 = CARTESIAN_POINT ( 'NONE',  ( -294.9999999999999432, -95.00000000000008527, 30.00000000000002842 ) ) ;
#7607 = DIRECTION ( 'NONE',  ( -0.000000000000000000, -0.000000000000000000, -1.000000000000000000 ) ) ;
#7608 = ORIENTED_EDGE ( 'NONE', *, *, #12859, .F. ) ;
#7609 = FACE_OUTER_BOUND ( 'NONE', #7414, .T. ) ;
#7610 = CARTESIAN_POINT ( 'NONE',  ( 0.9586399445693629673, -0.5150000000000024558, 0.8293189044373063812 ) ) ;
#7611 = CARTESIAN_POINT ( 'NONE',  ( 0.2500000000000002220, 0.000000000000000000, 0.000000000000000000 ) ) ;
#7612 = DIRECTION ( 'NONE',  ( -0.000000000000000000, 1.000000000000000000, -0.000000000000000000 ) ) ;
#7613 =( NAMED_UNIT ( * ) SI_UNIT ( $, .STERADIAN. ) SOLID_ANGLE_UNIT ( ) );
#7614 = CARTESIAN_POINT ( 'NONE',  ( 8.673617379884035472E-16, 4.618802153517012954, 0.000000000000000000 ) ) ;
#7615 = EDGE_CURVE ( 'NONE', #2215, #6940, #4196, .T. ) ;
#7616 = ITEM_DEFINED_TRANSFORMATION ( 'NONE', 'NONE', #5372,  #14039 ) ;
#7617 = DIRECTION ( 'NONE',  ( 1.000000000000000000, 0.000000000000000000, 0.000000000000000000 ) ) ;
#7618 = EDGE_CURVE ( 'NONE', #2842, #10535, #5036, .T. ) ;
#7619 = ORIENTED_EDGE ( 'NONE', *, *, #4556, .T. ) ;
#7620 = VERTEX_POINT ( 'NONE', #12967 ) ;
#7621 = DIRECTION ( 'NONE',  ( -1.000000000000000000, 0.000000000000000000, 0.000000000000000000 ) ) ;
#7622 = ORIENTED_EDGE ( 'NONE', *, *, #6614, .F. ) ;
#7623 = LINE ( 'NONE', #1077, #11877 ) ;
#7624 = CIRCLE ( 'NONE', #5321, 5.500000000000005329 ) ;
#7625 = ORIENTED_EDGE ( 'NONE', *, *, #5179, .F. ) ;
#7626 = ORIENTED_EDGE ( 'NONE', *, *, #12517, .T. ) ;
#7627 = DIRECTION ( 'NONE',  ( -0.000000000000000000, -0.000000000000000000, 1.000000000000000000 ) ) ;
#7628 = ORIENTED_EDGE ( 'NONE', *, *, #10987, .T. ) ;
#7629 = AXIS2_PLACEMENT_3D ( 'NONE', #6974, #7117, #2630 ) ;
#7630 = CARTESIAN_POINT ( 'NONE',  ( 140.0000000000000000, -75.00000000000008527, 190.0000000000000000 ) ) ;
#7631 = DIRECTION ( 'NONE',  ( -0.000000000000000000, 1.000000000000000000, -0.000000000000000000 ) ) ;
#7632 = DIRECTION ( 'NONE',  ( 0.000000000000000000, 1.000000000000000000, 0.000000000000000000 ) ) ;
#7633 = DIRECTION ( 'NONE',  ( 0.000000000000000000, 0.000000000000000000, 1.000000000000000000 ) ) ;
#7634 = AXIS2_PLACEMENT_3D ( 'NONE', #7583, #2212, #5631 ) ;
#7635 = EDGE_CURVE ( 'NONE', #4565, #7668, #13127, .T. ) ;
#7636 = EDGE_CURVE ( 'NONE', #12690, #794, #7454, .T. ) ;
#7637 = DIRECTION ( 'NONE',  ( -0.000000000000000000, -1.000000000000000000, -0.000000000000000000 ) ) ;
#7638 = PRODUCT_DEFINITION_SHAPE ( 'NONE', 'NONE',  #14330 ) ;
#7639 = VERTEX_POINT ( 'NONE', #11888 ) ;
#7640 = VECTOR ( 'NONE', #525, 1000.000000000000000 ) ;
#7641 = ORIENTED_EDGE ( 'NONE', *, *, #1427, .T. ) ;
#7642 = DIRECTION ( 'NONE',  ( 0.000000000000000000, -1.224646799147353207E-16, 1.000000000000000000 ) ) ;
#7643 = ORIENTED_EDGE ( 'NONE', *, *, #7790, .T. ) ;
#7644 = CARTESIAN_POINT ( 'NONE',  ( -3.349226789952655547, -2.685125164760744809, -0.2236248678334863682 ) ) ;
#7645 = CARTESIAN_POINT ( 'NONE',  ( 2.740000000000000213, 0.9838866223910001096, -0.5150000000000001243 ) ) ;
#7646 = ADVANCED_FACE ( 'NONE', ( #12892 ), #11956, .F. ) ;
#7647 = ADVANCED_FACE ( 'NONE', ( #3115 ), #8393, .T. ) ;
#7648 = LINE ( 'NONE', #12083, #3211 ) ;
#7649 = VECTOR ( 'NONE', #9529, 1000.000000000000000 ) ;
#7650 = VERTEX_POINT ( 'NONE', #4125 ) ;
#7651 = ADVANCED_FACE ( 'NONE', ( #13101 ), #899, .F. ) ;
#7652 = CARTESIAN_POINT ( 'NONE',  ( 2.500000000000000000, 1.178949249685213863, -2.042000000000001148 ) ) ;
#7653 = AXIS2_PLACEMENT_3D ( 'NONE', #4645, #3486, #7954 ) ;
#7654 = CARTESIAN_POINT ( 'NONE',  ( 0.000000000000000000, 0.000000000000000000, -186.0000000000000000 ) ) ;
#7655 = CARTESIAN_POINT ( 'NONE',  ( -302.3499999999999659, 45.00000000000001421, 30.00000000000000000 ) ) ;
#7656 = ORIENTED_EDGE ( 'NONE', *, *, #7667, .F. ) ;
#7657 = ORIENTED_EDGE ( 'NONE', *, *, #10621, .T. ) ;
#7658 = CARTESIAN_POINT ( 'NONE',  ( 0.3226060873438401089, 2.189154565102731098, -0.5150000000000000133 ) ) ;
#7659 = AXIS2_PLACEMENT_3D ( 'NONE', #10478, #12643, #12508 ) ;
#7660 = CARTESIAN_POINT ( 'NONE',  ( 0.000000000000000000, 0.000000000000000000, -0.2800830152838844622 ) ) ;
#7661 = ORIENTED_EDGE ( 'NONE', *, *, #1553, .F. ) ;
#7662 = DIRECTION ( 'NONE',  ( -0.000000000000000000, -0.000000000000000000, 1.000000000000000000 ) ) ;
#7663 = AXIS2_PLACEMENT_3D ( 'NONE', #5988, #2650, #4693 ) ;
#7664 = LINE ( 'NONE', #12101, #13186 ) ;
#7665 = DIRECTION ( 'NONE',  ( 0.000000000000000000, 0.000000000000000000, 1.000000000000000000 ) ) ;
#7666 = AXIS2_PLACEMENT_3D ( 'NONE', #13227, #5674, #4386 ) ;
#7667 = EDGE_CURVE ( 'NONE', #13016, #2624, #3188, .T. ) ;
#7668 = VERTEX_POINT ( 'NONE', #5359 ) ;
#7669 = CARTESIAN_POINT ( 'NONE',  ( 20.55500000000001748, 0.000000000000000000, 2.500000000000000888 ) ) ;
#7670 = VECTOR ( 'NONE', #11723, 1000.000000000000000 ) ;
#7671 = ORIENTED_EDGE ( 'NONE', *, *, #7206, .T. ) ;
#7672 = DIRECTION ( 'NONE',  ( -0.8571673013836870192, 1.049727191973306873E-16, 0.5150380737757234151 ) ) ;
#7673 = PLANE ( 'NONE',  #3026 ) ;
#7674 =( GEOMETRIC_REPRESENTATION_CONTEXT ( 3 ) GLOBAL_UNCERTAINTY_ASSIGNED_CONTEXT ( ( #1588 ) ) GLOBAL_UNIT_ASSIGNED_CONTEXT ( ( #2896, #1941, #9573 ) ) REPRESENTATION_CONTEXT ( 'NONE', 'WORKASPACE' ) );
#7675 = EDGE_LOOP ( 'NONE', ( #2819, #8630 ) ) ;
#7676 = ORIENTED_EDGE ( 'NONE', *, *, #6558, .T. ) ;
#7677 = DIRECTION ( 'NONE',  ( -2.312964634635743450E-16, -1.000000000000000000, 0.000000000000000000 ) ) ;
#7678 = UNCERTAINTY_MEASURE_WITH_UNIT (LENGTH_MEASURE( 1.000000000000000082E-05 ), #10513, 'distance_accuracy_value', 'NONE');
#7679 = CARTESIAN_POINT ( 'NONE',  ( -5.000000000000000888, 8.660254037844390851, 200.0000000000000000 ) ) ;
#7680 = DIRECTION ( 'NONE',  ( 0.8949343913984707521, 0.000000000000000000, -0.4461977533473793223 ) ) ;
#7681 = DIRECTION ( 'NONE',  ( 0.000000000000000000, -1.000000000000000000, 0.000000000000000000 ) ) ;
#7682 = CARTESIAN_POINT ( 'NONE',  ( 17.00000000000000000, 0.000000000000000000, 2.055000000000000160 ) ) ;
#7683 = CARTESIAN_POINT ( 'NONE',  ( 0.000000000000000000, 0.000000000000000000, -210.0000000000000000 ) ) ;
#7684 = AXIS2_PLACEMENT_3D ( 'NONE', #6744, #1433, #3618 ) ;
#7685 = CARTESIAN_POINT ( 'NONE',  ( -314.9999999999999432, 55.00000000000001421, 40.00000000000000000 ) ) ;
#7686 = CARTESIAN_POINT ( 'NONE',  ( 124.9999999999999858, 55.00000000000000711, 10.00000000000000000 ) ) ;
#7687 = AXIS2_PLACEMENT_3D ( 'NONE', #6519, #7738, #11014 ) ;
#7688 = ORIENTED_EDGE ( 'NONE', *, *, #5967, .F. ) ;
#7689 = AXIS2_PLACEMENT_3D ( 'NONE', #13283, #9881, #6401 ) ;
#7690 = ORIENTED_EDGE ( 'NONE', *, *, #11720, .F. ) ;
#7691 = CARTESIAN_POINT ( 'NONE',  ( 236.4999999999999432, -85.00000000000007105, 180.0000000000000000 ) ) ;
#7692 = ORIENTED_EDGE ( 'NONE', *, *, #8451, .F. ) ;
#7693 = DIRECTION ( 'NONE',  ( 0.000000000000000000, 0.000000000000000000, 1.000000000000000000 ) ) ;
#7694 = ORIENTED_EDGE ( 'NONE', *, *, #12414, .T. ) ;
#7695 = AXIS2_PLACEMENT_3D ( 'NONE', #13809, #11500, #8301 ) ;
#7696 = ORIENTED_EDGE ( 'NONE', *, *, #5243, .T. ) ;
#7697 = CARTESIAN_POINT ( 'NONE',  ( 347.0000000000000000, -8.660254037844389075, 199.9990000000000236 ) ) ;
#7698 = VERTEX_POINT ( 'NONE', #14119 ) ;
#7699 = EDGE_CURVE ( 'NONE', #4974, #8960, #3975, .T. ) ;
#7700 = CARTESIAN_POINT ( 'NONE',  ( 203.5000000000000000, -85.00000000000007105, 190.0000000000000000 ) ) ;
#7701 = CARTESIAN_POINT ( 'NONE',  ( 197.5000000000000000, -80.00000000000007105, 50.00000000000001421 ) ) ;
#7702 = CARTESIAN_POINT ( 'NONE',  ( 137.6499999999999488, -36.99999999999997868, 10.00000000000000000 ) ) ;
#7703 = FACE_OUTER_BOUND ( 'NONE', #2257, .T. ) ;
#7704 = AXIS2_PLACEMENT_3D ( 'NONE', #3562, #11534, #9363 ) ;
#7705 = FACE_OUTER_BOUND ( 'NONE', #1407, .T. ) ;
#7706 =( REPRESENTATION_RELATIONSHIP ('NONE','NONE', #11251, #208 ) REPRESENTATION_RELATIONSHIP_WITH_TRANSFORMATION ( #5521 )SHAPE_REPRESENTATION_RELATIONSHIP( ) );
#7707 = CARTESIAN_POINT ( 'NONE',  ( -31.74999999999995737, 0.000000000000000000, 4.250000000000000000 ) ) ;
#7708 = DIRECTION ( 'NONE',  ( 0.000000000000000000, 0.000000000000000000, -1.000000000000000000 ) ) ;
#7709 = VECTOR ( 'NONE', #13296, 1000.000000000000000 ) ;
#7710 = ORIENTED_EDGE ( 'NONE', *, *, #7014, .F. ) ;
#7711 = ORIENTED_EDGE ( 'NONE', *, *, #10587, .T. ) ;
#7712 = ADVANCED_FACE ( 'NONE', ( #10218 ), #14208, .F. ) ;
#7713 = DIRECTION ( 'NONE',  ( 1.000000000000000000, 0.000000000000000000, 0.000000000000000000 ) ) ;
#7714 = VERTEX_POINT ( 'NONE', #5218 ) ;
#7715 = DIRECTION ( 'NONE',  ( -1.000000000000000000, 0.000000000000000000, 0.000000000000000000 ) ) ;
#7716 = ADVANCED_FACE ( 'NONE', ( #2083 ), #2007, .F. ) ;
#7717 = DIRECTION ( 'NONE',  ( 0.000000000000000000, -0.000000000000000000, 1.000000000000000000 ) ) ;
#7718 = PRODUCT_RELATED_PRODUCT_CATEGORY ( 'part', '', ( #13394 ) ) ;
#7719 = PRESENTATION_STYLE_ASSIGNMENT (( #13241 ) ) ;
#7720 = ORIENTED_EDGE ( 'NONE', *, *, #14290, .F. ) ;
#7721 = CARTESIAN_POINT ( 'NONE',  ( 0.2500000000000002220, 0.000000000000000000, 0.000000000000000000 ) ) ;
#7722 = CARTESIAN_POINT ( 'NONE',  ( -299.9999999999999432, -75.00000000000008527, 354.1421356237308942 ) ) ;
#7723 = CARTESIAN_POINT ( 'NONE',  ( -31.74999999999995737, 0.000000000000000000, 4.250000000000000000 ) ) ;
#7724 = PRODUCT_DEFINITION_SHAPE ( 'NONE', 'NONE',  #13657 ) ;
#7725 = CARTESIAN_POINT ( 'NONE',  ( 2.500000000000000000, 2.357898499370431722, -2.818925648462311528E-15 ) ) ;
#7726 = EDGE_CURVE ( 'NONE', #3475, #1918, #8460, .T. ) ;
#7727 = ADVANCED_FACE ( 'NONE', ( #4267 ), #3865, .F. ) ;
#7728 = ORIENTED_EDGE ( 'NONE', *, *, #2055, .T. ) ;
#7729 = CARTESIAN_POINT ( 'NONE',  ( 142.6500000000000057, -75.00000000000008527, -186.2999999999999829 ) ) ;
#7730 = SHAPE_REPRESENTATION ( 'axis', ( #14039 ), #4938 ) ;
#7731 = DIRECTION ( 'NONE',  ( 0.000000000000000000, 0.000000000000000000, -1.000000000000000000 ) ) ;
#7732 = ADVANCED_FACE ( 'NONE', ( #8684 ), #12029, .F. ) ;
#7733 = CARTESIAN_POINT ( 'NONE',  ( 4.999999999999999112, -8.660254037844389075, 199.9990000000000236 ) ) ;
#7734 = ORIENTED_EDGE ( 'NONE', *, *, #7699, .T. ) ;
#7735 = DIRECTION ( 'NONE',  ( -0.000000000000000000, -0.000000000000000000, -1.000000000000000000 ) ) ;
#7736 = DIRECTION ( 'NONE',  ( 0.000000000000000000, 0.000000000000000000, -1.000000000000000000 ) ) ;
#7737 = DIRECTION ( 'NONE',  ( -0.000000000000000000, -0.000000000000000000, 1.000000000000000000 ) ) ;
#7738 = DIRECTION ( 'NONE',  ( -1.000000000000000000, 0.000000000000000000, 0.000000000000000000 ) ) ;
#7739 = EDGE_CURVE ( 'NONE', #13503, #2327, #10800, .T. ) ;
#7740 = VECTOR ( 'NONE', #4348, 1000.000000000000000 ) ;
#7741 = ORIENTED_EDGE ( 'NONE', *, *, #9332, .T. ) ;
#7742 = DIRECTION ( 'NONE',  ( 0.000000000000000000, 0.000000000000000000, -1.000000000000000000 ) ) ;
#7743 = ORIENTED_EDGE ( 'NONE', *, *, #8229, .F. ) ;
#7744 = LINE ( 'NONE', #1273, #7222 ) ;
#7745 = EDGE_CURVE ( 'NONE', #3306, #11114, #6221, .T. ) ;
#7746 = EDGE_LOOP ( 'NONE', ( #13920, #5323, #8770, #8354 ) ) ;
#7747 = VERTEX_POINT ( 'NONE', #5150 ) ;
#7748 = CARTESIAN_POINT ( 'NONE',  ( 2.500000000000000000, 1.178949249685213863, -2.042000000000001148 ) ) ;
#7749 = LINE ( 'NONE', #12179, #8037 ) ;
#7750 = DIRECTION ( 'NONE',  ( -0.000000000000000000, -0.000000000000000000, 1.000000000000000000 ) ) ;
#7751 = LINE ( 'NONE', #45, #8306 ) ;
#7752 = DIRECTION ( 'NONE',  ( 0.000000000000000000, 1.000000000000000000, -1.471414886128461471E-15 ) ) ;
#7753 = CARTESIAN_POINT ( 'NONE',  ( 319.9999999999999432, -20.00000000000000000, -19.99999999999998934 ) ) ;
#7754 =( LENGTH_UNIT ( ) NAMED_UNIT ( * ) SI_UNIT ( .MILLI., .METRE. ) );
#7755 = CARTESIAN_POINT ( 'NONE',  ( -6.259644161404860030E-16, -4.618802153517027165, -3.433295621305388234 ) ) ;
#7756 = CARTESIAN_POINT ( 'NONE',  ( -140.0000000000000000, -95.00000000000008527, 30.00000000000000000 ) ) ;
#7757 = ORIENTED_EDGE ( 'NONE', *, *, #8640, .T. ) ;
#7758 = ORIENTED_EDGE ( 'NONE', *, *, #6587, .F. ) ;
#7759 = DIRECTION ( 'NONE',  ( -0.000000000000000000, -0.000000000000000000, 1.000000000000000000 ) ) ;
#7760 = AXIS2_PLACEMENT_3D ( 'NONE', #7312, #9360, #13770 ) ;
#7761 = VERTEX_POINT ( 'NONE', #355 ) ;
#7762 = CARTESIAN_POINT ( 'NONE',  ( 299.9999999999999432, -95.00000000000008527, -190.0000000000000000 ) ) ;
#7763 = EDGE_LOOP ( 'NONE', ( #9768, #14181, #12229, #11557 ) ) ;
#7764 = DIRECTION ( 'NONE',  ( -1.000000000000000000, -0.000000000000000000, -0.000000000000000000 ) ) ;
#7765 = ORIENTED_EDGE ( 'NONE', *, *, #9443, .T. ) ;
#7766 = CARTESIAN_POINT ( 'NONE',  ( 4.000000000000000000, 2.309401076758497151, -3.433295621305379353 ) ) ;
#7767 = CARTESIAN_POINT ( 'NONE',  ( 305.4999999999999432, -95.00000000000008527, 190.0000000000000000 ) ) ;
#7768 =( NAMED_UNIT ( * ) SI_UNIT ( $, .STERADIAN. ) SOLID_ANGLE_UNIT ( ) );
#7769 = ADVANCED_FACE ( 'NONE', ( #8883 ), #3660, .F. ) ;
#7770 = CARTESIAN_POINT ( 'NONE',  ( -6.473970235329672780E-16, -4.862606272033106691, -3.745885042887442395 ) ) ;
#7771 = CIRCLE ( 'NONE', #322, 2.649999999999985700 ) ;
#7772 = CIRCLE ( 'NONE', #1506, 0.2000000000000022593 ) ;
#7773 = CARTESIAN_POINT ( 'NONE',  ( 0.000000000000000000, 0.000000000000000000, -4.000000000000000000 ) ) ;
#7774 = ORIENTED_EDGE ( 'NONE', *, *, #10658, .F. ) ;
#7775 = ORIENTED_EDGE ( 'NONE', *, *, #758, .T. ) ;
#7776 = LINE ( 'NONE', #5545, #7709 ) ;
#7777 = CIRCLE ( 'NONE', #8235, 2.649999999999985700 ) ;
#7778 = ORIENTED_EDGE ( 'NONE', *, *, #6048, .T. ) ;
#7779 = CARTESIAN_POINT ( 'NONE',  ( -144.9999999999999432, 55.00000000000001421, 30.00000000000000000 ) ) ;
#7780 = CARTESIAN_POINT ( 'NONE',  ( 0.000000000000000000, 1.178949249685212974, -2.042000000000001148 ) ) ;
#7781 = VECTOR ( 'NONE', #10147, 1000.000000000000000 ) ;
#7782 = DIRECTION ( 'NONE',  ( -0.000000000000000000, -0.000000000000000000, -1.000000000000000000 ) ) ;
#7783 = ORIENTED_EDGE ( 'NONE', *, *, #8134, .T. ) ;
#7784 = VECTOR ( 'NONE', #1556, 1000.000000000000000 ) ;
#7785 = FACE_OUTER_BOUND ( 'NONE', #1148, .T. ) ;
#7786 = LINE ( 'NONE', #2288, #10690 ) ;
#7787 = VECTOR ( 'NONE', #7202, 1000.000000000000000 ) ;
#7788 = DIRECTION ( 'NONE',  ( -0.000000000000000000, 1.000000000000000000, -0.000000000000000000 ) ) ;
#7789 = DIRECTION ( 'NONE',  ( 0.000000000000000000, 0.000000000000000000, 1.000000000000000000 ) ) ;
#7790 = EDGE_CURVE ( 'NONE', #4316, #12864, #2476, .T. ) ;
#7791 = VECTOR ( 'NONE', #8887, 1000.000000000000000 ) ;
#7792 = ORIENTED_EDGE ( 'NONE', *, *, #1377, .F. ) ;
#7793 = EDGE_CURVE ( 'NONE', #10596, #9721, #2223, .T. ) ;
#7794 = AXIS2_PLACEMENT_3D ( 'NONE', #3382, #12217, #5683 ) ;
#7795 = DIRECTION ( 'NONE',  ( 0.000000000000000000, 0.000000000000000000, -1.000000000000000000 ) ) ;
#7796 = VECTOR ( 'NONE', #14230, 1000.000000000000000 ) ;
#7797 = ORIENTED_EDGE ( 'NONE', *, *, #12675, .T. ) ;
#7798 = PLANE ( 'NONE',  #7569 ) ;
#7799 = AXIS2_PLACEMENT_3D ( 'NONE', #9820, #8936, #10090 ) ;
#7800 = DIRECTION ( 'NONE',  ( -0.000000000000000000, -0.000000000000000000, 1.000000000000000000 ) ) ;
#7801 = CARTESIAN_POINT ( 'NONE',  ( -314.9999999999999432, -105.0000000000000995, 30.00000000000000000 ) ) ;
#7802 = DIRECTION ( 'NONE',  ( 1.000000000000000000, 0.000000000000000000, 0.000000000000000000 ) ) ;
#7803 = VECTOR ( 'NONE', #3953, 1000.000000000000000 ) ;
#7804 = EDGE_CURVE ( 'NONE', #6598, #7398, #3727, .T. ) ;
#7805 = EDGE_CURVE ( 'NONE', #5615, #3295, #14045, .T. ) ;
#7806=STYLED_ITEM('',(#14403),#8473);
#7807 = ORIENTED_EDGE ( 'NONE', *, *, #10581, .T. ) ;
#7808 = CIRCLE ( 'NONE', #13600, 0.2000000000000022593 ) ;
#7809 = DIRECTION ( 'NONE',  ( -0.000000000000000000, -1.000000000000000000, -0.000000000000000000 ) ) ;
#7810 = ORIENTED_EDGE ( 'NONE', *, *, #4395, .T. ) ;
#7811 = FACE_OUTER_BOUND ( 'NONE', #11235, .T. ) ;
#7812 = ORIENTED_EDGE ( 'NONE', *, *, #13849, .T. ) ;
#7813 = EDGE_LOOP ( 'NONE', ( #12804, #2379, #14201, #12130, #5475 ) ) ;
#7814 = LINE ( 'NONE', #12253, #10808 ) ;
#7815 = EDGE_CURVE ( 'NONE', #14007, #2814, #1118, .T. ) ;
#7816 = EDGE_CURVE ( 'NONE', #12343, #4511, #2071, .T. ) ;
#7817 = VECTOR ( 'NONE', #6151, 1000.000000000000000 ) ;
#7818 = CARTESIAN_POINT ( 'NONE',  ( 219.9999999999999716, -85.00000000000007105, 55.00000000000002132 ) ) ;
#7819 = DIRECTION ( 'NONE',  ( 1.000000000000000000, 0.000000000000000000, 0.000000000000000000 ) ) ;
#7820 = EDGE_CURVE ( 'NONE', #13737, #5507, #992, .T. ) ;
#7821 = EDGE_CURVE ( 'NONE', #12252, #10809, #8736, .T. ) ;
#7822 = AXIS2_PLACEMENT_3D ( 'NONE', #12293, #6, #4471 ) ;
#7823 = CARTESIAN_POINT ( 'NONE',  ( 0.000000000000000000, -1.178949249685213863, 2.042000000000002924 ) ) ;
#7824 = CARTESIAN_POINT ( 'NONE',  ( 2.740000000000000213, -0.5150000000000022338, 0.6774776749089210792 ) ) ;
#7825 = CARTESIAN_POINT ( 'NONE',  ( 134.9999999999999432, -36.99999999999997868, -180.0000000000000000 ) ) ;
#7826 = DIRECTION ( 'NONE',  ( 1.000000000000000000, 0.000000000000000000, -0.000000000000000000 ) ) ;
#7827 = ADVANCED_FACE ( 'NONE', ( #2573 ), #24, .F. ) ;
#7828 = FACE_OUTER_BOUND ( 'NONE', #8060, .T. ) ;
#7829 = ORIENTED_EDGE ( 'NONE', *, *, #214, .T. ) ;
#7830 = ORIENTED_EDGE ( 'NONE', *, *, #6336, .T. ) ;
#7831 = VECTOR ( 'NONE', #3850, 1000.000000000000000 ) ;
#7832 = CARTESIAN_POINT ( 'NONE',  ( 219.9999999999999716, -14.99999999999999822, 222.5000000000000853 ) ) ;
#7833 = ORIENTED_EDGE ( 'NONE', *, *, #7993, .F. ) ;
#7834 = LINE ( 'NONE', #11187, #13484 ) ;
#7835 = ORIENTED_EDGE ( 'NONE', *, *, #6590, .F. ) ;
#7836 = CARTESIAN_POINT ( 'NONE',  ( -20.63749999999999574, 1.524685264938454646E-15, 12.44999999999999929 ) ) ;
#7837 = EDGE_LOOP ( 'NONE', ( #13485, #6311 ) ) ;
#7838 = CARTESIAN_POINT ( 'NONE',  ( 2.500000000000000000, 2.357898499370433054, -1.951563910473907981E-15 ) ) ;
#7839 = PRODUCT ( 'vertical suport', 'vertical suport', '', ( #12701 ) ) ;
#7840 = DIRECTION ( 'NONE',  ( -1.000000000000000000, 0.000000000000000000, 0.000000000000000000 ) ) ;
#7841 = CARTESIAN_POINT ( 'NONE',  ( 2.500000000000000000, 3.004629197474318851E-15, 2.042000000000000259 ) ) ;
#7842 = CARTESIAN_POINT ( 'NONE',  ( 305.4999999999999432, -75.00000000000008527, 190.0000000000000000 ) ) ;
#7843 = SHAPE_REPRESENTATION_RELATIONSHIP ( 'NONE' , 'NONE' ,  #208, #7317 ) ;
#7844 = DIRECTION ( 'NONE',  ( 6.123233995736766036E-17, 0.000000000000000000, -1.000000000000000000 ) ) ;
#7845 = FACE_BOUND ( 'NONE', #320, .T. ) ;
#7846 = ORIENTED_EDGE ( 'NONE', *, *, #10987, .F. ) ;
#7847 = AXIS2_PLACEMENT_3D ( 'NONE', #6446, #1940, #4201 ) ;
#7848 = VERTEX_POINT ( 'NONE', #5491 ) ;
#7849 = ADVANCED_FACE ( 'NONE', ( #974 ), #7798, .T. ) ;
#7850 = DIRECTION ( 'NONE',  ( 0.000000000000000000, 0.000000000000000000, 1.000000000000000000 ) ) ;
#7851 = EDGE_LOOP ( 'NONE', ( #3675, #7676, #9514, #14293 ) ) ;
#7852 = DIRECTION ( 'NONE',  ( 0.000000000000000000, 0.000000000000000000, 1.000000000000000000 ) ) ;
#7853 = CARTESIAN_POINT ( 'NONE',  ( -30.00000000000002842, -25.00000000000000000, -169.9999999999999716 ) ) ;
#7854 = DIRECTION ( 'NONE',  ( 1.000000000000000000, 0.000000000000000000, 0.000000000000000000 ) ) ;
#7855 = AXIS2_PLACEMENT_3D ( 'NONE', #8010, #4767, #1481 ) ;
#7856 = FACE_OUTER_BOUND ( 'NONE', #9650, .T. ) ;
#7857 = VECTOR ( 'NONE', #10791, 1000.000000000000000 ) ;
#7858 = CARTESIAN_POINT ( 'NONE',  ( 434.9999999999999432, 8.660254037844390851, 200.0000000000000000 ) ) ;
#7859 = CARTESIAN_POINT ( 'NONE',  ( 136.6666666666666288, -25.00000000000000000, -222.5000000000000853 ) ) ;
#7860 = CARTESIAN_POINT ( 'NONE',  ( 124.9999999999999858, 55.00000000000000711, 0.000000000000000000 ) ) ;
#7861 = VERTEX_POINT ( 'NONE', #1195 ) ;
#7862 = DIRECTION ( 'NONE',  ( -0.000000000000000000, -0.000000000000000000, -1.000000000000000000 ) ) ;
#7863 = AXIS2_PLACEMENT_3D ( 'NONE', #4137, #9725, #8554 ) ;
#7864 = FACE_OUTER_BOUND ( 'NONE', #2097, .T. ) ;
#7865 = DIRECTION ( 'NONE',  ( 0.000000000000000000, 0.000000000000000000, 1.000000000000000000 ) ) ;
#7866 = AXIS2_PLACEMENT_3D ( 'NONE', #11912, #1959, #6392 ) ;
#7867 = EDGE_LOOP ( 'NONE', ( #10468, #5166, #13279, #8632 ) ) ;
#7868 = EDGE_CURVE ( 'NONE', #9652, #4280, #10590, .T. ) ;
#7869 = DIRECTION ( 'NONE',  ( -1.000000000000000000, 0.000000000000000000, 0.000000000000000000 ) ) ;
#7870 = CARTESIAN_POINT ( 'NONE',  ( 0.2500000000000002220, 0.000000000000000000, 0.000000000000000000 ) ) ;
#7871 = CARTESIAN_POINT ( 'NONE',  ( 439.9999999999999432, 0.000000000000000000, 0.000000000000000000 ) ) ;
#7872 = CIRCLE ( 'NONE', #7907, 4.250000000000000000 ) ;
#7873 = AXIS2_PLACEMENT_3D ( 'NONE', #14052, #7457, #11892 ) ;
#7874 = ORIENTED_EDGE ( 'NONE', *, *, #7093, .T. ) ;
#7875 = LINE ( 'NONE', #5574, #12175 ) ;
#7876 = ORIENTED_EDGE ( 'NONE', *, *, #7232, .F. ) ;
#7877 = CARTESIAN_POINT ( 'NONE',  ( 2.807080416178989513, -3.225969019225150003, -3.502507215260505014 ) ) ;
#7878 = VECTOR ( 'NONE', #1622, 1000.000000000000000 ) ;
#7879 = VERTEX_POINT ( 'NONE', #9848 ) ;
#7880 = ORIENTED_EDGE ( 'NONE', *, *, #3434, .T. ) ;
#7882 = ADVANCED_FACE ( 'NONE', ( #10324 ), #5426, .F. ) ;
#7881 = DIRECTION ( 'NONE',  ( 1.000000000000000000, 0.000000000000000000, 0.000000000000000000 ) ) ;
#7883 = CARTESIAN_POINT ( 'NONE',  ( 259.0000000000000000, 8.660254037844390851, 200.0000000000000000 ) ) ;
#7884 = CARTESIAN_POINT ( 'NONE',  ( 236.4999999999999432, -85.00000000000007105, 180.0000000000000000 ) ) ;
#7885 = AXIS2_PLACEMENT_3D ( 'NONE', #7497, #4089, #3161 ) ;
#7886 = DIRECTION ( 'NONE',  ( -0.000000000000000000, -0.000000000000000000, 1.000000000000000000 ) ) ;
#7887 = DIRECTION ( 'NONE',  ( 0.000000000000000000, 0.000000000000000000, -1.000000000000000000 ) ) ;
#7888 = CARTESIAN_POINT ( 'NONE',  ( 2.500000000000000000, 2.357898499370433054, -1.951563910473907981E-15 ) ) ;
#7889 = DIRECTION ( 'NONE',  ( -0.000000000000000000, -0.000000000000000000, 1.000000000000000000 ) ) ;
#7890 = ITEM_DEFINED_TRANSFORMATION ( 'NONE', 'NONE', #5159,  #14039 ) ;
#7891 = VECTOR ( 'NONE', #11141, 1000.000000000000000 ) ;
#7892 = ORIENTED_EDGE ( 'NONE', *, *, #4353, .F. ) ;
#7893 = VERTEX_POINT ( 'NONE', #13182 ) ;
#7894 = EDGE_CURVE ( 'NONE', #12590, #1452, #2941, .T. ) ;
#7895 = EDGE_CURVE ( 'NONE', #3696, #11791, #2159, .T. ) ;
#7896 = DIRECTION ( 'NONE',  ( 1.000000000000000000, 0.000000000000000000, 0.000000000000000000 ) ) ;
#7897 = ORIENTED_EDGE ( 'NONE', *, *, #6771, .F. ) ;
#7898 = ADVANCED_FACE ( 'NONE', ( #10474 ), #4095, .F. ) ;
#7899 = LINE ( 'NONE', #13551, #5841 ) ;
#7900 = EDGE_LOOP ( 'NONE', ( #10516, #2829, #6706, #11124 ) ) ;
#7901 = DIRECTION ( 'NONE',  ( -0.000000000000000000, -0.000000000000000000, -1.000000000000000000 ) ) ;
#7902 = VERTEX_POINT ( 'NONE', #7347 ) ;
#7903 = CARTESIAN_POINT ( 'NONE',  ( 0.000000000000000000, 0.000000000000000000, -5.000000000000000000 ) ) ;
#7904 = CARTESIAN_POINT ( 'NONE',  ( 294.4999999999999432, -75.00000000000008527, 186.2999999999999829 ) ) ;
#7905 = VECTOR ( 'NONE', #10016, 1000.000000000000000 ) ;
#7906 = DIRECTION ( 'NONE',  ( 0.000000000000000000, 0.000000000000000000, 1.000000000000000000 ) ) ;
#7907 = AXIS2_PLACEMENT_3D ( 'NONE', #6076, #12533, #13898 ) ;
#7908 = DIRECTION ( 'NONE',  ( 0.000000000000000000, 0.000000000000000000, 1.000000000000000000 ) ) ;
#7909 = AXIS2_PLACEMENT_3D ( 'NONE', #5642, #94, #10064 ) ;
#7910 = SURFACE_STYLE_FILL_AREA ( #6623 ) ;
#7911 = DIRECTION ( 'NONE',  ( -0.000000000000000000, -0.000000000000000000, 1.000000000000000000 ) ) ;
#7912 = APPLICATION_PROTOCOL_DEFINITION ( 'draft international standard', 'automotive_design', 1998, #7578 ) ;
#7913 = LINE ( 'NONE', #6978, #7122 ) ;
#7914 = ORIENTED_EDGE ( 'NONE', *, *, #7373, .F. ) ;
#7915 = VERTEX_POINT ( 'NONE', #5979 ) ;
#7916 = EDGE_CURVE ( 'NONE', #247, #11681, #11053, .T. ) ;
#7917 = ORIENTED_EDGE ( 'NONE', *, *, #1350, .T. ) ;
#7918 = DIRECTION ( 'NONE',  ( 0.000000000000000000, 0.000000000000000000, -1.000000000000000000 ) ) ;
#7919 = AXIS2_PLACEMENT_3D ( 'NONE', #13970, #817, #5209 ) ;
#7920 = PRESENTATION_LAYER_ASSIGNMENT (  '', '', ( #8148 ) ) ;
#7921 = EDGE_LOOP ( 'NONE', ( #8051, #1698 ) ) ;
#7922 = DIRECTION ( 'NONE',  ( 0.000000000000000000, 0.000000000000000000, -1.000000000000000000 ) ) ;
#7923 = DIRECTION ( 'NONE',  ( -0.000000000000000000, 1.000000000000000000, -0.000000000000000000 ) ) ;
#7924 = DIRECTION ( 'NONE',  ( -0.000000000000000000, -0.000000000000000000, 1.000000000000000000 ) ) ;
#7926 = AXIS2_PLACEMENT_3D ( 'NONE', #6319, #1957, #5237 ) ;
#7925 = AXIS2_PLACEMENT_3D ( 'NONE', #811, #9696, #14103 ) ;
#7927 = CARTESIAN_POINT ( 'NONE',  ( -124.9999999999999432, -105.0000000000000853, 40.00000000000000000 ) ) ;
#7928 = CARTESIAN_POINT ( 'NONE',  ( -5.000000000000000888, 8.660254037844390851, 199.9990000000000236 ) ) ;
#7929 = ORIENTED_EDGE ( 'NONE', *, *, #8902, .T. ) ;
#7930 = DIRECTION ( 'NONE',  ( -1.000000000000000000, -0.000000000000000000, -0.000000000000000000 ) ) ;
#7931 =( GEOMETRIC_REPRESENTATION_CONTEXT ( 3 ) GLOBAL_UNCERTAINTY_ASSIGNED_CONTEXT ( ( #3206 ) ) GLOBAL_UNIT_ASSIGNED_CONTEXT ( ( #12844, #8708, #7613 ) ) REPRESENTATION_CONTEXT ( 'NONE', 'WORKASPACE' ) );
#7932 = CARTESIAN_POINT ( 'NONE',  ( 299.9999999999999432, -95.00000000000008527, -190.0000000000000000 ) ) ;
#7933 = ORIENTED_EDGE ( 'NONE', *, *, #10050, .F. ) ;
#7934 = CIRCLE ( 'NONE', #7487, 5.500000000000005329 ) ;
#7935 = CARTESIAN_POINT ( 'NONE',  ( 13.50000000000000000, 1.653273178848926867E-15, -186.0000000000000000 ) ) ;
#7936 = CARTESIAN_POINT ( 'NONE',  ( -124.9999999999999432, 55.00000000000001421, 40.00000000000000000 ) ) ;
#7937 = LINE ( 'NONE', #13383, #14073 ) ;
#7938 = ORIENTED_EDGE ( 'NONE', *, *, #8445, .F. ) ;
#7939 = DIRECTION ( 'NONE',  ( 1.000000000000000000, 0.000000000000000000, 0.000000000000000000 ) ) ;
#7940 = ADVANCED_FACE ( 'NONE', ( #3872 ), #7275, .F. ) ;
#7941 = CARTESIAN_POINT ( 'NONE',  ( 0.000000000000000000, 2.357898499370431722, -2.818925648462311528E-15 ) ) ;
#7942 = DIRECTION ( 'NONE',  ( 6.123233995736766036E-17, -1.000000000000000000, 0.000000000000000000 ) ) ;
#7943 = EDGE_LOOP ( 'NONE', ( #7272, #12957 ) ) ;
#7944 = EDGE_CURVE ( 'NONE', #7098, #6925, #4323, .T. ) ;
#7945 = DIRECTION ( 'NONE',  ( -0.000000000000000000, -0.000000000000000000, 1.000000000000000000 ) ) ;
#7946 = PRODUCT ( 'roller axis', 'roller axis', '', ( #4810 ) ) ;
#7947 = EDGE_LOOP ( 'NONE', ( #8724, #6037, #4135, #4600 ) ) ;
#7948 = CARTESIAN_POINT ( 'NONE',  ( 0.6640947660595348800, -4.471078309994175548, -3.602146406945708090 ) ) ;
#7949 = ORIENTED_EDGE ( 'NONE', *, *, #11065, .F. ) ;
#7950 = ORIENTED_EDGE ( 'NONE', *, *, #968, .F. ) ;
#7951 = CARTESIAN_POINT ( 'NONE',  ( 2.500000000000000000, 1.178949249685217415, 2.041999999999998483 ) ) ;
#7952 = DIRECTION ( 'NONE',  ( -0.000000000000000000, -0.000000000000000000, 1.000000000000000000 ) ) ;
#7953 = FACE_OUTER_BOUND ( 'NONE', #11758, .T. ) ;
#7954 = DIRECTION ( 'NONE',  ( -1.000000000000000000, 0.000000000000000000, 0.000000000000000000 ) ) ;
#7955 = CARTESIAN_POINT ( 'NONE',  ( 137.4999999999999432, -36.99999999999997868, -169.9999999999999716 ) ) ;
#7956 = LINE ( 'NONE', #10224, #2950 ) ;
#7957 = CARTESIAN_POINT ( 'NONE',  ( 0.000000000000000000, 0.000000000000000000, 190.0000000000000000 ) ) ;
#7958 = ITEM_DEFINED_TRANSFORMATION ( 'NONE', 'NONE', #1421,  #14039 ) ;
#7959 = ORIENTED_EDGE ( 'NONE', *, *, #1342, .F. ) ;
#7960 = ORIENTED_EDGE ( 'NONE', *, *, #7194, .F. ) ;
#7961 = ADVANCED_FACE ( 'NONE', ( #7137, #9537, #2716, #1753, #6192, #657 ), #1686, .F. ) ;
#7962 = DIRECTION ( 'NONE',  ( 1.000000000000000000, 0.000000000000000000, 0.000000000000000000 ) ) ;
#7963 = EDGE_CURVE ( 'NONE', #1839, #12345, #10546, .T. ) ;
#7964 =( REPRESENTATION_RELATIONSHIP ('NONE','NONE', #11251, #5332 ) REPRESENTATION_RELATIONSHIP_WITH_TRANSFORMATION ( #7890 )SHAPE_REPRESENTATION_RELATIONSHIP( ) );
#7965 = ORIENTED_EDGE ( 'NONE', *, *, #6590, .T. ) ;
#7966 = CARTESIAN_POINT ( 'NONE',  ( 1.424271237134740131, -4.556291390728484991, -5.579847667638274858E-16 ) ) ;
#7967 = AXIS2_PLACEMENT_3D ( 'NONE', #6111, #12784, #6040 ) ;
#7968 = ORIENTED_EDGE ( 'NONE', *, *, #8444, .T. ) ;
#7969 = DIRECTION ( 'NONE',  ( 1.000000000000000000, 0.000000000000000000, 0.000000000000000000 ) ) ;
#7970 = ORIENTED_EDGE ( 'NONE', *, *, #7805, .F. ) ;
#7971 = PLANE ( 'NONE',  #10097 ) ;
#7972 = DIRECTION ( 'NONE',  ( 0.000000000000000000, 0.000000000000000000, -1.000000000000000000 ) ) ;
#7973 = EDGE_CURVE ( 'NONE', #924, #2940, #3793, .T. ) ;
#7974 = CARTESIAN_POINT ( 'NONE',  ( 470.0000000000000000, -25.00000000000000000, 250.0000000000000000 ) ) ;
#7975 = FILL_AREA_STYLE_COLOUR ( '', #13713 ) ;
#7976 = CARTESIAN_POINT ( 'NONE',  ( 299.9999999999999432, -75.00000000000008527, 190.0000000000000000 ) ) ;
#7977 = CYLINDRICAL_SURFACE ( 'NONE', #8511, 2.500000000000002220 ) ;
#7978 = ORIENTED_EDGE ( 'NONE', *, *, #12352, .F. ) ;
#7979 = VECTOR ( 'NONE', #13447, 1000.000000000000000 ) ;
#7980 = ADVANCED_FACE ( 'NONE', ( #508 ), #8290, .F. ) ;
#7981 = ORIENTED_EDGE ( 'NONE', *, *, #1323, .F. ) ;
#7982 = ORIENTED_EDGE ( 'NONE', *, *, #2503, .F. ) ;
#7983 = FACE_OUTER_BOUND ( 'NONE', #136, .T. ) ;
#7984 = VERTEX_POINT ( 'NONE', #11781 ) ;
#7985 = CARTESIAN_POINT ( 'NONE',  ( 0.000000000000000000, 0.000000000000000000, -4.694516984716113228 ) ) ;
#7986 = VERTEX_POINT ( 'NONE', #12720 ) ;
#7987 = DIRECTION ( 'NONE',  ( 0.000000000000000000, -1.000000000000000000, 0.000000000000000000 ) ) ;
#7988 = AXIS2_PLACEMENT_3D ( 'NONE', #7903, #1084, #1301 ) ;
#7989 = CARTESIAN_POINT ( 'NONE',  ( 319.9999999999999432, -225.0010000000000048, 169.9999999999999716 ) ) ;
#7990 = VECTOR ( 'NONE', #2445, 1000.000000000000000 ) ;
#7991 = EDGE_CURVE ( 'NONE', #11776, #145, #13732, .T. ) ;
#7992 = DIRECTION ( 'NONE',  ( -1.000000000000000000, -0.000000000000000000, -0.000000000000000000 ) ) ;
#7993 = EDGE_CURVE ( 'NONE', #8297, #11341, #1833, .T. ) ;
#7994 = CARTESIAN_POINT ( 'NONE',  ( 4.000000000001088907, 1.658577278524410170, -3.531553309554541720 ) ) ;
#7995 = DIRECTION ( 'NONE',  ( 1.000000000000000000, 0.000000000000000000, 0.000000000000000000 ) ) ;
#7996 = DIRECTION ( 'NONE',  ( 0.000000000000000000, 0.000000000000000000, -1.000000000000000000 ) ) ;
#7997 = EDGE_CURVE ( 'NONE', #8807, #3312, #5268, .T. ) ;
#7998 = ORIENTED_EDGE ( 'NONE', *, *, #12376, .F. ) ;
#7999 = VECTOR ( 'NONE', #12465, 1000.000000000000000 ) ;
#8001 = VECTOR ( 'NONE', #7952, 1000.000000000000000 ) ;
#8000 =( LENGTH_UNIT ( ) NAMED_UNIT ( * ) SI_UNIT ( .MILLI., .METRE. ) );
#8002 = CYLINDRICAL_SURFACE ( 'NONE', #12525, 2.649999999999985700 ) ;
#8003 = CARTESIAN_POINT ( 'NONE',  ( -20.63749999999999929, 0.000000000000000000, 0.000000000000000000 ) ) ;
#8004 = DIRECTION ( 'NONE',  ( -0.000000000000000000, -0.000000000000000000, -1.000000000000000000 ) ) ;
#8005 = AXIS2_PLACEMENT_3D ( 'NONE', #12264, #5852, #2739 ) ;
#8006 = VERTEX_POINT ( 'NONE', #12796 ) ;
#8007 = AXIS2_PLACEMENT_3D ( 'NONE', #9462, #11706, #5044 ) ;
#8008 = CARTESIAN_POINT ( 'NONE',  ( 299.9999999999999432, -75.00000000000008527, -190.0000000000000000 ) ) ;
#8009 = AXIS2_PLACEMENT_3D ( 'NONE', #10995, #3242, #7715 ) ;
#8010 = CARTESIAN_POINT ( 'NONE',  ( 2.500000000000000000, 0.000000000000000000, 0.000000000000000000 ) ) ;
#8011 = DIRECTION ( 'NONE',  ( 0.000000000000000000, 0.000000000000000000, 1.000000000000000000 ) ) ;
#8012 = EDGE_CURVE ( 'NONE', #8933, #4585, #6880, .T. ) ;
#8013 = VECTOR ( 'NONE', #12607, 1000.000000000000000 ) ;
#8014 = ORIENTED_EDGE ( 'NONE', *, *, #10729, .F. ) ;
#8015 = CARTESIAN_POINT ( 'NONE',  ( 1.799999999999996048, 0.000000000000000000, 0.000000000000000000 ) ) ;
#8016 = PRESENTATION_LAYER_ASSIGNMENT (  '', '', ( #12667 ) ) ;
#8017 = VERTEX_POINT ( 'NONE', #428 ) ;
#8018 = EDGE_CURVE ( 'NONE', #3584, #5681, #4897, .T. ) ;
#8019 = CARTESIAN_POINT ( 'NONE',  ( 386.6666666666666288, -20.00000000000000000, 219.8500000000001080 ) ) ;
#8020 = CIRCLE ( 'NONE', #7571, 2.649999999999985700 ) ;
#8021 = AXIS2_PLACEMENT_3D ( 'NONE', #1303, #9297, #3784 ) ;
#8022 = EDGE_LOOP ( 'NONE', ( #3100, #13074, #6702, #12220 ) ) ;
#8023 = ORIENTED_EDGE ( 'NONE', *, *, #9419, .T. ) ;
#8024 = DIRECTION ( 'NONE',  ( -1.000000000000000000, 0.000000000000000000, 0.000000000000000000 ) ) ;
#8025 = CARTESIAN_POINT ( 'NONE',  ( 0.5449313310647804220, 4.304185902836899835, -3.316620875263383894 ) ) ;
#8026 = AXIS2_PLACEMENT_3D ( 'NONE', #2997, #3933, #13787 ) ;
#8027 =( REPRESENTATION_RELATIONSHIP ('NONE','NONE', #11251, #2740 ) REPRESENTATION_RELATIONSHIP_WITH_TRANSFORMATION ( #10682 )SHAPE_REPRESENTATION_RELATIONSHIP( ) );
#8028 = FILL_AREA_STYLE_COLOUR ( '', #10848 ) ;
#8029 = DIRECTION ( 'NONE',  ( 0.000000000000000000, 0.000000000000000000, 1.000000000000000000 ) ) ;
#8030 = CIRCLE ( 'NONE', #13371, 2.700000000000001066 ) ;
#8031 = DIRECTION ( 'NONE',  ( -0.000000000000000000, -0.000000000000000000, 1.000000000000000000 ) ) ;
#8032 = LINE ( 'NONE', #13618, #14278 ) ;
#8033 =( LENGTH_UNIT ( ) NAMED_UNIT ( * ) SI_UNIT ( .MILLI., .METRE. ) );
#8034 = CARTESIAN_POINT ( 'NONE',  ( 4.197393957002303999, 7.772902908466098641E-14, -3.503767560748929810 ) ) ;
#8035 = CONTEXT_DEPENDENT_SHAPE_REPRESENTATION ( #2800, #10651 ) ;
#8036 = AXIS2_PLACEMENT_3D ( 'NONE', #4546, #1116, #2297 ) ;
#8037 = VECTOR ( 'NONE', #10890, 1000.000000000000000 ) ;
#8038 = VERTEX_POINT ( 'NONE', #8874 ) ;
#8039 = ORIENTED_EDGE ( 'NONE', *, *, #1399, .T. ) ;
#8040 = DIRECTION ( 'NONE',  ( 0.000000000000000000, 1.000000000000000000, 0.000000000000000000 ) ) ;
#8041 = EDGE_CURVE ( 'NONE', #4959, #8189, #1910, .T. ) ;
#8042 = AXIS2_PLACEMENT_3D ( 'NONE', #11841, #13932, #8418 ) ;
#8043 = EDGE_LOOP ( 'NONE', ( #5893, #7192, #13242, #4529 ) ) ;
#8044 = LINE ( 'NONE', #12404, #3314 ) ;
#8045 = ORIENTED_EDGE ( 'NONE', *, *, #2918, .F. ) ;
#8046 = DIRECTION ( 'NONE',  ( 0.000000000000000000, 1.000000000000000000, 0.000000000000000000 ) ) ;
#8047 = EDGE_LOOP ( 'NONE', ( #8499, #395, #1319, #8261, #3776 ) ) ;
#8048 = FACE_OUTER_BOUND ( 'NONE', #11101, .T. ) ;
#8049 = AXIS2_PLACEMENT_3D ( 'NONE', #5756, #7924, #3383 ) ;
#8050 = DIRECTION ( 'NONE',  ( 0.000000000000000000, 0.000000000000000000, -1.000000000000000000 ) ) ;
#8051 = ORIENTED_EDGE ( 'NONE', *, *, #10592, .T. ) ;
#8052 = EDGE_CURVE ( 'NONE', #3648, #13411, #5538, .T. ) ;
#8053 = DIRECTION ( 'NONE',  ( -0.000000000000000000, 1.000000000000000000, -0.000000000000000000 ) ) ;
#8054 =( NAMED_UNIT ( * ) PLANE_ANGLE_UNIT ( ) SI_UNIT ( $, .RADIAN. ) );
#8055 = FACE_OUTER_BOUND ( 'NONE', #4287, .T. ) ;
#8056 = SHAPE_DEFINITION_REPRESENTATION ( #8076, #10314 ) ;
#8057 = CARTESIAN_POINT ( 'NONE',  ( 469.9999999999998863, -225.0000000000000000, -169.9999999999999716 ) ) ;
#8058 = ORIENTED_EDGE ( 'NONE', *, *, #11290, .T. ) ;
#8059 = VECTOR ( 'NONE', #10323, 1000.000000000000000 ) ;
#8060 = EDGE_LOOP ( 'NONE', ( #6778, #7657, #11410, #5466 ) ) ;
#8061 = ORIENTED_EDGE ( 'NONE', *, *, #4837, .F. ) ;
#8062 = CIRCLE ( 'NONE', #7375, 2.500000000000000444 ) ;
#8063 = DIRECTION ( 'NONE',  ( 0.000000000000000000, 0.000000000000000000, 1.000000000000000000 ) ) ;
#8064 = ORIENTED_EDGE ( 'NONE', *, *, #2589, .T. ) ;
#8065 = DIRECTION ( 'NONE',  ( 1.000000000000000000, 0.000000000000000000, 0.000000000000000000 ) ) ;
#8066 = EDGE_LOOP ( 'NONE', ( #5621, #7211, #12066, #8773 ) ) ;
#8067 = CARTESIAN_POINT ( 'NONE',  ( 5.000000000000002665, 3.306546357697854226E-16, 2.700000000000000622 ) ) ;
#8068 = CARTESIAN_POINT ( 'NONE',  ( 0.7826237921249277196, 0.000000000000000000, 0.000000000000000000 ) ) ;
#8070 = EDGE_CURVE ( 'NONE', #3366, #4821, #2127, .T. ) ;
#8069 = VECTOR ( 'NONE', #2197, 1000.000000000000114 ) ;
#8071 = EDGE_CURVE ( 'NONE', #7639, #10296, #11999, .T. ) ;
#8072 = CARTESIAN_POINT ( 'NONE',  ( 434.9999999999999432, 8.660254037844390851, 205.0000000000000284 ) ) ;
#8073 = CARTESIAN_POINT ( 'NONE',  ( -5.000000000000000888, 8.660254037844390851, -210.0000000000000000 ) ) ;
#8074 = AXIS2_PLACEMENT_3D ( 'NONE', #5155, #12899, #7523 ) ;
#8075 = CARTESIAN_POINT ( 'NONE',  ( 305.0000000000000000, -56.99999999999997158, -180.0000000000000000 ) ) ;
#8076 = PRODUCT_DEFINITION_SHAPE ( 'NONE', 'NONE',  #8892 ) ;
#8077 = DIRECTION ( 'NONE',  ( 0.000000000000000000, 0.000000000000000000, -1.000000000000000000 ) ) ;
#8078 = ORIENTED_EDGE ( 'NONE', *, *, #9646, .T. ) ;
#8079 = EDGE_CURVE ( 'NONE', #7668, #8946, #12210, .T. ) ;
#8080 = EDGE_CURVE ( 'NONE', #14219, #13531, #6428, .T. ) ;
#8081 = ADVANCED_FACE ( 'NONE', ( #9824 ), #6620, .T. ) ;
#8082 = CARTESIAN_POINT ( 'NONE',  ( -2.688821387764050996E-14, -4.618802153517012954, -0.4999999999999995559 ) ) ;
#8083 = CARTESIAN_POINT ( 'NONE',  ( 357.0000000000000000, -8.660254037844389075, 200.0000000000000000 ) ) ;
#8084 = DIRECTION ( 'NONE',  ( -0.000000000000000000, -0.000000000000000000, -1.000000000000000000 ) ) ;
#8085 = ORIENTED_EDGE ( 'NONE', *, *, #1597, .F. ) ;
#8086 = AXIS2_PLACEMENT_3D ( 'NONE', #2074, #12089, #9915 ) ;
#8087 = DIRECTION ( 'NONE',  ( 1.000000000000000000, 0.000000000000000000, 0.000000000000000000 ) ) ;
#8088 = FACE_OUTER_BOUND ( 'NONE', #10231, .T. ) ;
#8089 = DIRECTION ( 'NONE',  ( 0.000000000000000000, 0.000000000000000000, -1.000000000000000000 ) ) ;
#8090 = CIRCLE ( 'NONE', #2778, 2.500000000000000888 ) ;
#8091 = PLANE ( 'NONE',  #4555 ) ;
#8092 = AXIS2_PLACEMENT_3D ( 'NONE', #9347, #2743, #4850 ) ;
#8093 = CIRCLE ( 'NONE', #5782, 4.250000000000000000 ) ;
#8094 = VERTEX_POINT ( 'NONE', #3231 ) ;
#8095 = PLANE ( 'NONE',  #2545 ) ;
#8096 = AXIS2_PLACEMENT_3D ( 'NONE', #3643, #9373, #9226 ) ;
#8097 = CARTESIAN_POINT ( 'NONE',  ( 469.9999999999998863, -225.0000000000000000, -169.9999999999999716 ) ) ;
#8098 = ORIENTED_EDGE ( 'NONE', *, *, #3658, .T. ) ;
#8099 = VERTEX_POINT ( 'NONE', #798 ) ;
#8100 = CARTESIAN_POINT ( 'NONE',  ( -1.800000000000001155, 0.000000000000000000, 0.000000000000000000 ) ) ;
#8101 = CARTESIAN_POINT ( 'NONE',  ( 0.1410422978106145031, -4.700232962125109104, -3.687027686973628704 ) ) ;
#8102 = DIRECTION ( 'NONE',  ( 0.000000000000000000, 0.000000000000000000, -1.000000000000000000 ) ) ;
#8103 = CARTESIAN_POINT ( 'NONE',  ( -5.000000000000000888, 8.660254037844390851, -210.0000000000000000 ) ) ;
#8104 = DIRECTION ( 'NONE',  ( 0.000000000000000000, 0.000000000000000000, 1.000000000000000000 ) ) ;
#8105 = PLANE ( 'NONE',  #593 ) ;
#8106 = SURFACE_STYLE_USAGE ( .BOTH. , #468 ) ;
#8107 = EDGE_CURVE ( 'NONE', #1904, #6772, #870, .T. ) ;
#8108 = CIRCLE ( 'NONE', #680, 10.00000000000000888 ) ;
#8109 = CARTESIAN_POINT ( 'NONE',  ( 222.4999999999999147, -85.00000000000009948, -17.55500000000000327 ) ) ;
#8110 = ITEM_DEFINED_TRANSFORMATION ( 'NONE', 'NONE', #8147,  #14039 ) ;
#8111 = VERTEX_POINT ( 'NONE', #13223 ) ;
#8112 = ORIENTED_EDGE ( 'NONE', *, *, #10137, .F. ) ;
#8113 = FACE_OUTER_BOUND ( 'NONE', #8022, .T. ) ;
#8114 = VECTOR ( 'NONE', #8682, 1000.000000000000000 ) ;
#8115 = VERTEX_POINT ( 'NONE', #6481 ) ;
#8116 = LINE ( 'NONE', #11324, #28 ) ;
#8117 = ORIENTED_EDGE ( 'NONE', *, *, #10763, .T. ) ;
#8118 = CARTESIAN_POINT ( 'NONE',  ( 4.999999999999999112, 8.660254037844390851, 210.0000000000000000 ) ) ;
#8119 = ORIENTED_EDGE ( 'NONE', *, *, #603, .F. ) ;
#8120 = DIRECTION ( 'NONE',  ( 1.000000000000000000, 0.000000000000000000, 0.000000000000000000 ) ) ;
#8121 = DIRECTION ( 'NONE',  ( -0.000000000000000000, -0.000000000000000000, -1.000000000000000000 ) ) ;
#8122 = ORIENTED_EDGE ( 'NONE', *, *, #13322, .F. ) ;
#8123 = PRESENTATION_STYLE_ASSIGNMENT (( #13636 ) ) ;
#8124 = CARTESIAN_POINT ( 'NONE',  ( 79.99999999999971578, 35.00000000000000000, 0.000000000000000000 ) ) ;
#8125 = VECTOR ( 'NONE', #11490, 1000.000000000000000 ) ;
#8126 = DIRECTION ( 'NONE',  ( 0.000000000000000000, -1.000000000000000000, 1.287488025362403787E-15 ) ) ;
#8127 = APPLICATION_PROTOCOL_DEFINITION ( 'draft international standard', 'automotive_design', 1998, #12581 ) ;
#8128 = FACE_BOUND ( 'NONE', #1023, .T. ) ;
#8129 = ORIENTED_EDGE ( 'NONE', *, *, #9818, .F. ) ;
#8130 = CIRCLE ( 'NONE', #8365, 2.649999999999985700 ) ;
#8131 = ORIENTED_EDGE ( 'NONE', *, *, #11656, .F. ) ;
#8132 = ORIENTED_EDGE ( 'NONE', *, *, #11575, .T. ) ;
#8133 = DIRECTION ( 'NONE',  ( -0.8571673013836870192, 1.049727191973306873E-16, 0.5150380737757234151 ) ) ;
#8134 = EDGE_CURVE ( 'NONE', #7902, #9721, #14305, .T. ) ;
#8135 = AXIS2_PLACEMENT_3D ( 'NONE', #6992, #11425, #1467 ) ;
#8136 = VERTEX_POINT ( 'NONE', #3299 ) ;
#8137 = DIRECTION ( 'NONE',  ( -0.000000000000000000, 1.471414886128461471E-15, 1.000000000000000000 ) ) ;
#8138 = VERTEX_POINT ( 'NONE', #1088 ) ;
#8139 = CARTESIAN_POINT ( 'NONE',  ( 0.000000000000000000, 0.000000000000000000, 40.00000000000000000 ) ) ;
#8140 = LINE ( 'NONE', #2499, #8059 ) ;
#8141 = DIRECTION ( 'NONE',  ( 0.000000000000000000, 0.000000000000000000, 1.000000000000000000 ) ) ;
#8142 = LINE ( 'NONE', #12582, #8125 ) ;
#8143 = CARTESIAN_POINT ( 'NONE',  ( 0.9586399445693771781, -0.5149999999999964606, -0.8293189044373090457 ) ) ;
#8144 = AXIS2_PLACEMENT_3D ( 'NONE', #8221, #6132, #7070 ) ;
#8145 = CARTESIAN_POINT ( 'NONE',  ( -4.000000000000000000, 2.309401076758498483, -5.000000000000000000 ) ) ;
#8146 = ORIENTED_EDGE ( 'NONE', *, *, #4522, .T. ) ;
#8147 = AXIS2_PLACEMENT_3D ( 'NONE', #11301, #5777, #4705 ) ;
#8148 = STYLED_ITEM ( 'NONE', ( #13758 ), #13210 ) ;
#8149 = VECTOR ( 'NONE', #194, 1000.000000000000000 ) ;
#8150 = EDGE_CURVE ( 'NONE', #7188, #4208, #6346, .T. ) ;
#8151 = PRODUCT_DEFINITION ( 'UNKNOWN', '', #500, #10454 ) ;
#8152 = CARTESIAN_POINT ( 'NONE',  ( -294.9999999999999432, -65.00000000000011369, 40.00000000000000000 ) ) ;
#8153 = CARTESIAN_POINT ( 'NONE',  ( 0.000000000000000000, 0.5149999999999917977, 2.350000000000001865 ) ) ;
#8154 = VECTOR ( 'NONE', #12806, 1000.000000000000000 ) ;
#8155 = CARTESIAN_POINT ( 'NONE',  ( -140.0000000000000000, -75.00000000000008527, -14.14213562373090127 ) ) ;
#8156 = EDGE_CURVE ( 'NONE', #5131, #10596, #11932, .T. ) ;
#8157 = VERTEX_POINT ( 'NONE', #8728 ) ;
#8158 = CIRCLE ( 'NONE', #4165, 9.999999999999980460 ) ;
#8159 = CARTESIAN_POINT ( 'NONE',  ( 144.9999999999999716, -64.99999999999997158, 10.00000000000000000 ) ) ;
#8160 = ADVANCED_FACE ( 'NONE', ( #13150 ), #8267, .T. ) ;
#8161 = EDGE_CURVE ( 'NONE', #12143, #11802, #10770, .T. ) ;
#8162 = CARTESIAN_POINT ( 'NONE',  ( 136.6666666666666288, -20.00000000000000000, -222.5000000000000853 ) ) ;
#8163 = DIRECTION ( 'NONE',  ( 1.000000000000000000, 0.000000000000000000, 0.000000000000000000 ) ) ;
#8164 = FACE_OUTER_BOUND ( 'NONE', #820, .T. ) ;
#8165 = AXIS2_PLACEMENT_3D ( 'NONE', #3099, #14099, #10854 ) ;
#8166 = EDGE_LOOP ( 'NONE', ( #8862, #5787, #11870, #1550 ) ) ;
#8167 = EDGE_CURVE ( 'NONE', #5643, #6568, #6409, .T. ) ;
#8168 = FACE_OUTER_BOUND ( 'NONE', #9897, .T. ) ;
#8169 = DIRECTION ( 'NONE',  ( -1.000000000000000000, 0.000000000000000000, -0.000000000000000000 ) ) ;
#8170 = ORIENTED_EDGE ( 'NONE', *, *, #11962, .F. ) ;
#8171 = LINE ( 'NONE', #11519, #5700 ) ;
#8172 = CARTESIAN_POINT ( 'NONE',  ( 170.9999999999999716, 8.660254037844390851, 205.0000000000000284 ) ) ;
#8173 = CARTESIAN_POINT ( 'NONE',  ( 82.99999999999998579, -8.660254037844389075, 205.0000000000000284 ) ) ;
#8174 = ADVANCED_FACE ( 'NONE', ( #7703 ), #7496, .T. ) ;
#8175 = CARTESIAN_POINT ( 'NONE',  ( 134.5000000000000000, -75.00000000000008527, -186.2999999999999829 ) ) ;
#8176 = PLANE ( 'NONE',  #1062 ) ;
#8177 = EDGE_CURVE ( 'NONE', #1098, #5839, #7426, .T. ) ;
#8178 = CARTESIAN_POINT ( 'NONE',  ( -137.6499999999999773, 45.00000000000001421, 30.00000000000000000 ) ) ;
#8179 = CONTEXT_DEPENDENT_SHAPE_REPRESENTATION ( #10027, #9613 ) ;
#8180 = ORIENTED_EDGE ( 'NONE', *, *, #8367, .T. ) ;
#8181 = ORIENTED_EDGE ( 'NONE', *, *, #5187, .T. ) ;
#8182 = ADVANCED_FACE ( 'NONE', ( #11858 ), #13012, .F. ) ;
#8183 = CYLINDRICAL_SURFACE ( 'NONE', #9628, 5.000000000000004441 ) ;
#8184 = VERTEX_POINT ( 'NONE', #2554 ) ;
#8185 = PLANE ( 'NONE',  #11202 ) ;
#8186 = DIRECTION ( 'NONE',  ( 0.4461977533474923430, 3.124646727056501017E-15, -0.8949343913984144638 ) ) ;
#8187 = EDGE_LOOP ( 'NONE', ( #12635, #12104, #14047 ) ) ;
#8188 = CARTESIAN_POINT ( 'NONE',  ( 219.9999999999999716, -20.00000000000000000, -222.5000000000000853 ) ) ;
#8189 = VERTEX_POINT ( 'NONE', #3638 ) ;
#8190 = DIRECTION ( 'NONE',  ( -0.000000000000000000, -0.000000000000000000, -1.000000000000000000 ) ) ;
#8191 = PRODUCT_DEFINITION_SHAPE ( 'NONE', 'NONE',  #14327 ) ;
#8192 = LINE ( 'NONE', #7112, #1778 ) ;
#8193 = VERTEX_POINT ( 'NONE', #7841 ) ;
#8194 = CARTESIAN_POINT ( 'NONE',  ( 2.500000000000000000, -2.357898499370432610, 3.252606517456513302E-15 ) ) ;
#8195 = DIRECTION ( 'NONE',  ( 1.000000000000000000, 0.000000000000000000, 0.000000000000000000 ) ) ;
#8196 = FILL_AREA_STYLE ('',( #411 ) ) ;
#8197 =( NAMED_UNIT ( * ) PLANE_ANGLE_UNIT ( ) SI_UNIT ( $, .RADIAN. ) );
#8198 = PRODUCT_CONTEXT ( 'NONE', #11561, 'mechanical' ) ;
#8199 = CARTESIAN_POINT ( 'NONE',  ( 236.4999999999999432, -85.00000000000007105, 190.0000000000000000 ) ) ;
#8200 = ORIENTED_EDGE ( 'NONE', *, *, #2773, .F. ) ;
#8201 = ORIENTED_EDGE ( 'NONE', *, *, #13625, .F. ) ;
#8202 = ORIENTED_EDGE ( 'NONE', *, *, #6698, .T. ) ;
#8203 = CARTESIAN_POINT ( 'NONE',  ( -30.00000000000002842, 15.00000000000000000, 200.0000000000000000 ) ) ;
#8204 = EDGE_CURVE ( 'NONE', #2540, #4912, #9673, .T. ) ;
#8205 = EDGE_LOOP ( 'NONE', ( #11310, #13599, #3275, #7033 ) ) ;
#8206 = DIRECTION ( 'NONE',  ( 0.000000000000000000, 0.000000000000000000, 1.000000000000000000 ) ) ;
#8207 = ORIENTED_EDGE ( 'NONE', *, *, #8645, .F. ) ;
#8208 = CARTESIAN_POINT ( 'NONE',  ( 203.5000000000000000, -85.00000000000007105, 178.4978484569338946 ) ) ;
#8209 =( NAMED_UNIT ( * ) PLANE_ANGLE_UNIT ( ) SI_UNIT ( $, .RADIAN. ) );
#8210 = DIRECTION ( 'NONE',  ( -1.000000000000000000, 0.000000000000000000, 0.000000000000000000 ) ) ;
#8211 = VECTOR ( 'NONE', #5873, 1000.000000000000000 ) ;
#8212 = PLANE ( 'NONE',  #3298 ) ;
#8213 = CIRCLE ( 'NONE', #2906, 2.649999999999985700 ) ;
#8214 = DIRECTION ( 'NONE',  ( -0.000000000000000000, -0.000000000000000000, 1.000000000000000000 ) ) ;
#8215 = DIRECTION ( 'NONE',  ( -1.000000000000000000, 0.000000000000000000, -0.000000000000000000 ) ) ;
#8216 = ORIENTED_EDGE ( 'NONE', *, *, #13054, .F. ) ;
#8217 = ORIENTED_EDGE ( 'NONE', *, *, #4935, .F. ) ;
#8218 = CIRCLE ( 'NONE', #5684, 5.500000000000005329 ) ;
#8219 = ORIENTED_EDGE ( 'NONE', *, *, #2946, .F. ) ;
#8220 = CARTESIAN_POINT ( 'NONE',  ( 132.3499999999999659, -56.99999999999997158, 10.00000000000000178 ) ) ;
#8221 = CARTESIAN_POINT ( 'NONE',  ( 236.4999999999999432, -85.00000000000007105, 50.00000000000001421 ) ) ;
#8222 = FILL_AREA_STYLE_COLOUR ( '', #5983 ) ;
#8223 = ORIENTED_EDGE ( 'NONE', *, *, #1609, .F. ) ;
#8224 = DIRECTION ( 'NONE',  ( -0.000000000000000000, -0.000000000000000000, 1.000000000000000000 ) ) ;
#8225 = EDGE_CURVE ( 'NONE', #2418, #8279, #13142, .T. ) ;
#8226 = AXIS2_PLACEMENT_3D ( 'NONE', #5603, #13555, #2475 ) ;
#8227 = CARTESIAN_POINT ( 'NONE',  ( -314.9999999999999432, 55.00000000000001421, 40.00000000000000000 ) ) ;
#8228 = DIRECTION ( 'NONE',  ( 1.000000000000000000, 0.000000000000000000, 0.000000000000000000 ) ) ;
#8229 = EDGE_CURVE ( 'NONE', #13282, #4602, #7339, .T. ) ;
#8230 = CARTESIAN_POINT ( 'NONE',  ( 4.999999999999997335, 0.000000000000000000, 0.000000000000000000 ) ) ;
#8231 = LINE ( 'NONE', #11581, #12194 ) ;
#8232 = ORIENTED_EDGE ( 'NONE', *, *, #11033, .F. ) ;
#8233 = CARTESIAN_POINT ( 'NONE',  ( -4.000000000000000000, -2.309401076758512694, -3.433295621305382461 ) ) ;
#8234 = DIRECTION ( 'NONE',  ( -1.000000000000000000, 0.000000000000000000, 0.000000000000000000 ) ) ;
#8235 = AXIS2_PLACEMENT_3D ( 'NONE', #5509, #248, #103 ) ;
#8236 = VERTEX_POINT ( 'NONE', #13424 ) ;
#8237 = DIRECTION ( 'NONE',  ( 0.000000000000000000, 1.000000000000000000, 0.000000000000000000 ) ) ;
#8238 = VECTOR ( 'NONE', #9618, 1000.000000000000000 ) ;
#8239 =( NAMED_UNIT ( * ) PLANE_ANGLE_UNIT ( ) SI_UNIT ( $, .RADIAN. ) );
#8240 =( REPRESENTATION_RELATIONSHIP ('NONE','NONE', #11251, #13104 ) REPRESENTATION_RELATIONSHIP_WITH_TRANSFORMATION ( #763 )SHAPE_REPRESENTATION_RELATIONSHIP( ) );
#8241 = FILL_AREA_STYLE ('',( #388 ) ) ;
#8242 = EDGE_CURVE ( 'NONE', #14164, #7052, #14281, .T. ) ;
#8243 = PLANE ( 'NONE',  #2806 ) ;
#8244 = EDGE_CURVE ( 'NONE', #7372, #5306, #6650, .T. ) ;
#8245 = DIRECTION ( 'NONE',  ( -0.000000000000000000, -0.000000000000000000, -1.000000000000000000 ) ) ;
#8246 = CARTESIAN_POINT ( 'NONE',  ( 347.0000000000000000, 8.660254037844390851, 200.0000000000000000 ) ) ;
#8247 =( NAMED_UNIT ( * ) SI_UNIT ( $, .STERADIAN. ) SOLID_ANGLE_UNIT ( ) );
#8248 = AXIS2_PLACEMENT_3D ( 'NONE', #6536, #2321, #4505 ) ;
#8249 = CARTESIAN_POINT ( 'NONE',  ( 294.4999999999999432, -95.00000000000008527, 190.0000000000000000 ) ) ;
#8250 = CIRCLE ( 'NONE', #3661, 2.649999999999985700 ) ;
#8251 = EDGE_CURVE ( 'NONE', #13211, #9987, #10835, .T. ) ;
#8252 = ORIENTED_EDGE ( 'NONE', *, *, #12098, .T. ) ;
#8253 = CIRCLE ( 'NONE', #2724, 5.500000000000005329 ) ;
#8254 = DIRECTION ( 'NONE',  ( 0.000000000000000000, 0.000000000000000000, -1.000000000000000000 ) ) ;
#8255 = ORIENTED_EDGE ( 'NONE', *, *, #12515, .T. ) ;
#8256 = DIRECTION ( 'NONE',  ( -0.000000000000000000, -0.000000000000000000, 1.000000000000000000 ) ) ;
#8257 = DIRECTION ( 'NONE',  ( -0.000000000000000000, -0.000000000000000000, -1.000000000000000000 ) ) ;
#8258 = EDGE_CURVE ( 'NONE', #9549, #13517, #12348, .T. ) ;
#8259 = EDGE_CURVE ( 'NONE', #3648, #3584, #11991, .T. ) ;
#8260 = VECTOR ( 'NONE', #11558, 1000.000000000000000 ) ;
#8261 = ORIENTED_EDGE ( 'NONE', *, *, #2878, .T. ) ;
#8262 = EDGE_CURVE ( 'NONE', #9712, #3306, #14055, .T. ) ;
#8263 = CARTESIAN_POINT ( 'NONE',  ( 386.6666666666666288, -20.00000000000000000, -219.8500000000001080 ) ) ;
#8264 = ORIENTED_EDGE ( 'NONE', *, *, #11466, .T. ) ;
#8265 = EDGE_CURVE ( 'NONE', #12687, #8456, #5886, .T. ) ;
#8266 = CARTESIAN_POINT ( 'NONE',  ( 219.9999999999999716, -20.00000000000000000, -222.5000000000000853 ) ) ;
#8267 = TOROIDAL_SURFACE ( 'NONE', #11513, 4.300000000000001599, 0.4499999999999985678 ) ;
#8268 = CARTESIAN_POINT ( 'NONE',  ( 1.424271237134740131, 5.698459981794101142E-16, -4.556291390728477886 ) ) ;
#8269 = ORIENTED_EDGE ( 'NONE', *, *, #11039, .F. ) ;
#8270 = PRODUCT_DEFINITION_CONTEXT ( 'detailed design', #7578, 'design' ) ;
#8271 = DIRECTION ( 'NONE',  ( 0.000000000000000000, 0.000000000000000000, -1.000000000000000000 ) ) ;
#8272 = VECTOR ( 'NONE', #12159, 1000.000000000000114 ) ;
#8273 = CARTESIAN_POINT ( 'NONE',  ( 299.9999999999999432, -75.00000000000008527, 190.0000000000000000 ) ) ;
#8274 = AXIS2_PLACEMENT_3D ( 'NONE', #484, #3570, #12623 ) ;
#8275 = CARTESIAN_POINT ( 'NONE',  ( -5.000000000000000888, -8.660254037844389075, 205.0000000000000284 ) ) ;
#8276 = APPLICATION_PROTOCOL_DEFINITION ( 'draft international standard', 'automotive_design', 1998, #11561 ) ;
#8277 = DIRECTION ( 'NONE',  ( -1.000000000000000000, -0.000000000000000000, -0.000000000000000000 ) ) ;
#8278 = AXIS2_PLACEMENT_3D ( 'NONE', #8491, #9449, #645 ) ;
#8279 = VERTEX_POINT ( 'NONE', #5815 ) ;
#8280 = ORIENTED_EDGE ( 'NONE', *, *, #584, .T. ) ;
#8281 = ORIENTED_EDGE ( 'NONE', *, *, #871, .F. ) ;
#8282 = ORIENTED_EDGE ( 'NONE', *, *, #6735, .T. ) ;
#8283 = CARTESIAN_POINT ( 'NONE',  ( -5.000000000000000888, 8.660254037844390851, 210.0000000000000000 ) ) ;
#8284 = PRESENTATION_LAYER_ASSIGNMENT (  '', '', ( #159 ) ) ;
#8285 = ORIENTED_EDGE ( 'NONE', *, *, #5492, .T. ) ;
#8286 = FACE_OUTER_BOUND ( 'NONE', #13089, .T. ) ;
#8287 = ORIENTED_EDGE ( 'NONE', *, *, #11448, .T. ) ;
#8288 = DIRECTION ( 'NONE',  ( 0.000000000000000000, -0.000000000000000000, 1.000000000000000000 ) ) ;
#8289 = DIRECTION ( 'NONE',  ( 0.000000000000000000, -1.000000000000000000, 0.000000000000000000 ) ) ;
#8290 = CYLINDRICAL_SURFACE ( 'NONE', #1530, 2.649999999999985700 ) ;
#8291 = LINE ( 'NONE', #8072, #2587 ) ;
#8292 = CARTESIAN_POINT ( 'NONE',  ( 134.9999999999999716, 45.00000000000001421, 10.00000000000000000 ) ) ;
#8293 = MECHANICAL_DESIGN_GEOMETRIC_PRESENTATION_REPRESENTATION (  '', ( #159 ), #3664 ) ;
#8294 = CARTESIAN_POINT ( 'NONE',  ( 303.3333333333333144, -25.00000000000000000, 225.1500000000000625 ) ) ;
#8295 = ORIENTED_EDGE ( 'NONE', *, *, #12980, .F. ) ;
#8296 = EDGE_CURVE ( 'NONE', #9376, #278, #6902, .T. ) ;
#8297 = VERTEX_POINT ( 'NONE', #334 ) ;
#8298 = CARTESIAN_POINT ( 'NONE',  ( -3.999999999999999112, 1.539600717838996324, -3.300726591567078039 ) ) ;
#8299 = VERTEX_POINT ( 'NONE', #1304 ) ;
#8300 = DIRECTION ( 'NONE',  ( 1.000000000000000000, 0.000000000000000000, 0.000000000000000000 ) ) ;
#8301 = DIRECTION ( 'NONE',  ( 1.000000000000000000, 0.000000000000000000, 0.000000000000000000 ) ) ;
#8302 = SURFACE_SIDE_STYLE ('',( #11574 ) ) ;
#8303 = ORIENTED_EDGE ( 'NONE', *, *, #11930, .F. ) ;
#8304 = VECTOR ( 'NONE', #12330, 1000.000000000000000 ) ;
#8305 = CARTESIAN_POINT ( 'NONE',  ( 299.9999999999999432, -75.00000000000008527, 169.9999999999999716 ) ) ;
#8306 = VECTOR ( 'NONE', #12258, 1000.000000000000000 ) ;
#8307 = DIRECTION ( 'NONE',  ( -0.000000000000000000, -0.000000000000000000, 1.000000000000000000 ) ) ;
#8308 = CARTESIAN_POINT ( 'NONE',  ( 303.3333333333333144, -10.00000000000000178, -222.5000000000000853 ) ) ;
#8309 = CARTESIAN_POINT ( 'NONE',  ( 137.3500000000000227, -95.00000000000008527, 169.9999999999999716 ) ) ;
#8310 = DIRECTION ( 'NONE',  ( 0.000000000000000000, 1.000000000000000000, 0.000000000000000000 ) ) ;
#8311 = APPLICATION_CONTEXT ( 'automotive_design' ) ;
#8312 = ORIENTED_EDGE ( 'NONE', *, *, #13953, .F. ) ;
#8313 = AXIS2_PLACEMENT_3D ( 'NONE', #4986, #7443, #3029 ) ;
#8314 = CARTESIAN_POINT ( 'NONE',  ( -31.74999999999995737, 5.204748896376250699E-16, -4.250000000000000000 ) ) ;
#8315 = PRODUCT_DEFINITION_SHAPE ( 'NONE', 'NONE',  #14378 ) ;
#8316 = FACE_OUTER_BOUND ( 'NONE', #11716, .T. ) ;
#8317 = EDGE_CURVE ( 'NONE', #7714, #2336, #8500, .T. ) ;
#8318 = ORIENTED_EDGE ( 'NONE', *, *, #1250, .T. ) ;
#8319 = LINE ( 'NONE', #1426, #13573 ) ;
#8320 = SURFACE_STYLE_FILL_AREA ( #8241 ) ;
#8321 = CIRCLE ( 'NONE', #9263, 1.037871761867652065 ) ;
#8322 = CARTESIAN_POINT ( 'NONE',  ( 219.9999999999999147, -85.00000000000009948, 0.000000000000000000 ) ) ;
#8323 = FACE_OUTER_BOUND ( 'NONE', #4140, .T. ) ;
#8324 = CARTESIAN_POINT ( 'NONE',  ( 469.9999999999998863, -225.0000000000000000, -169.9999999999999716 ) ) ;
#8325 = VECTOR ( 'NONE', #15, 1000.000000000000000 ) ;
#8326 = DIRECTION ( 'NONE',  ( 0.000000000000000000, 0.000000000000000000, 1.000000000000000000 ) ) ;
#8327 = ORIENTED_EDGE ( 'NONE', *, *, #8715, .T. ) ;
#8328 = FACE_OUTER_BOUND ( 'NONE', #6684, .T. ) ;
#8329 = MANIFOLD_SOLID_BREP ( 'OuterRace', #10537 ) ;
#8330 = ORIENTED_EDGE ( 'NONE', *, *, #10135, .F. ) ;
#8331 = CARTESIAN_POINT ( 'NONE',  ( -294.9999999999999432, -105.0000000000000853, 30.00000000000000000 ) ) ;
#8332 = LINE ( 'NONE', #9506, #3326 ) ;
#8333 = EDGE_CURVE ( 'NONE', #2624, #1100, #6828, .T. ) ;
#8334 = PRODUCT_RELATED_PRODUCT_CATEGORY ( 'part', '', ( #3229 ) ) ;
#8335 = ORIENTED_EDGE ( 'NONE', *, *, #5865, .F. ) ;
#8336 = CARTESIAN_POINT ( 'NONE',  ( 347.0000000000000000, 8.660254037844390851, 205.0000000000000284 ) ) ;
#8337 = ORIENTED_EDGE ( 'NONE', *, *, #7991, .F. ) ;
#8338 = CARTESIAN_POINT ( 'NONE',  ( -302.4999999999999432, -75.00000000000008527, 10.00000000000000178 ) ) ;
#8339 = LINE ( 'NONE', #6168, #12920 ) ;
#8340 = ORIENTED_EDGE ( 'NONE', *, *, #1843, .T. ) ;
#8341 = CARTESIAN_POINT ( 'NONE',  ( 0.000000000000000000, -20.00000000000000000, 0.000000000000000000 ) ) ;
#8342 = VECTOR ( 'NONE', #6712, 1000.000000000000000 ) ;
#8343 = DIRECTION ( 'NONE',  ( 0.000000000000000000, 0.000000000000000000, 1.000000000000000000 ) ) ;
#8344 = CARTESIAN_POINT ( 'NONE',  ( 16.55500000000001393, 0.000000000000000000, 2.500000000000000444 ) ) ;
#8345 = SHAPE_DEFINITION_REPRESENTATION ( #1232, #208 ) ;
#8346 = EDGE_CURVE ( 'NONE', #794, #1872, #12841, .T. ) ;
#8347 = ADVANCED_FACE ( 'NONE', ( #487, #12773, #559, #3929, #9444, #12560 ), #13710, .F. ) ;
#8348 = LINE ( 'NONE', #7184, #4812 ) ;
#8349 = CIRCLE ( 'NONE', #13463, 2.499999999999999556 ) ;
#8350 = EDGE_LOOP ( 'NONE', ( #1544, #5772, #3413, #396 ) ) ;
#8351 = ADVANCED_FACE ( 'NONE', ( #6028 ), #8413, .F. ) ;
#8352 = ORIENTED_EDGE ( 'NONE', *, *, #11, .T. ) ;
#8353 = ORIENTED_EDGE ( 'NONE', *, *, #3752, .T. ) ;
#8354 = ORIENTED_EDGE ( 'NONE', *, *, #8701, .T. ) ;
#8355 = VECTOR ( 'NONE', #11352, 1000.000000000000000 ) ;
#8356 = CARTESIAN_POINT ( 'NONE',  ( 0.000000000000000000, -2.357898499370432610, 3.252606517456513302E-15 ) ) ;
#8357 = VERTEX_POINT ( 'NONE', #13925 ) ;
#8358 = DIRECTION ( 'NONE',  ( 1.110223024625157487E-14, 1.000000000000000000, 0.000000000000000000 ) ) ;
#8359 = VERTEX_POINT ( 'NONE', #3999 ) ;
#8360 = DIRECTION ( 'NONE',  ( -0.000000000000000000, -0.000000000000000000, -1.000000000000000000 ) ) ;
#8361 = DIRECTION ( 'NONE',  ( 0.000000000000000000, -0.000000000000000000, 1.000000000000000000 ) ) ;
#8362 = MANIFOLD_SOLID_BREP ( 'Mirror1', #9140 ) ;
#8363 = DIRECTION ( 'NONE',  ( -1.000000000000000000, 0.000000000000000000, 0.000000000000000000 ) ) ;
#8364 = DIRECTION ( 'NONE',  ( -1.000000000000000000, 0.000000000000000000, 0.000000000000000000 ) ) ;
#8365 = AXIS2_PLACEMENT_3D ( 'NONE', #412, #12700, #2771 ) ;
#8366 = DIRECTION ( 'NONE',  ( 1.000000000000000000, 1.460819769243627131E-16, 0.000000000000000000 ) ) ;
#8367 = EDGE_CURVE ( 'NONE', #8038, #3734, #2695, .T. ) ;
#8368 = VERTEX_POINT ( 'NONE', #3786 ) ;
#8369 = ORIENTED_EDGE ( 'NONE', *, *, #9018, .F. ) ;
#8370 = AXIS2_PLACEMENT_3D ( 'NONE', #10477, #9166, #10402 ) ;
#8371 = EDGE_CURVE ( 'NONE', #5737, #2276, #11614, .T. ) ;
#8372 = PLANE ( 'NONE',  #9803 ) ;
#8373 = STYLED_ITEM ( 'NONE', ( #13540 ), #6456 ) ;
#8374 = ORIENTED_EDGE ( 'NONE', *, *, #1428, .T. ) ;
#8375 = DIRECTION ( 'NONE',  ( -0.000000000000000000, -0.000000000000000000, 1.000000000000000000 ) ) ;
#8376 = CARTESIAN_POINT ( 'NONE',  ( 209.9999999999999716, -85.00000000000007105, 190.0000000000000000 ) ) ;
#8377 = VERTEX_POINT ( 'NONE', #1515 ) ;
#8378 = AXIS2_PLACEMENT_3D ( 'NONE', #9871, #8852, #11638 ) ;
#8379 = DIRECTION ( 'NONE',  ( -0.000000000000000000, -0.000000000000000000, 1.000000000000000000 ) ) ;
#8380 = AXIS2_PLACEMENT_3D ( 'NONE', #276, #10931, #9840 ) ;
#8381 = DIRECTION ( 'NONE',  ( 0.000000000000000000, 0.000000000000000000, 1.000000000000000000 ) ) ;
#8382 = DIRECTION ( 'NONE',  ( 1.000000000000000000, 2.775557561562891351E-17, 0.000000000000000000 ) ) ;
#8383 = DIRECTION ( 'NONE',  ( 1.000000000000000000, 6.123233995736766036E-17, -6.123233995736764803E-17 ) ) ;
#8384 = PLANE ( 'NONE',  #199 ) ;
#8385 = ORIENTED_EDGE ( 'NONE', *, *, #12946, .F. ) ;
#8386 = DIRECTION ( 'NONE',  ( -1.000000000000000000, -0.000000000000000000, -0.000000000000000000 ) ) ;
#8387 = VECTOR ( 'NONE', #8245, 1000.000000000000000 ) ;
#8388 = CARTESIAN_POINT ( 'NONE',  ( 0.000000000000000000, 0.000000000000000000, 55.00000000000001421 ) ) ;
#8389 = PRODUCT_DEFINITION_FORMATION_WITH_SPECIFIED_SOURCE ( 'ANY', '', #13394, .NOT_KNOWN. ) ;
#8390 = PRESENTATION_LAYER_ASSIGNMENT (  '', '', ( #10484 ) ) ;
#8391 = ADVANCED_FACE ( 'NONE', ( #640 ), #1784, .T. ) ;
#8392 = VERTEX_POINT ( 'NONE', #10607 ) ;
#8393 = CYLINDRICAL_SURFACE ( 'NONE', #8956, 10.00000000000000000 ) ;
#8394 = CARTESIAN_POINT ( 'NONE',  ( 21.00000000000000355, 2.516649172247811061E-16, -2.055000000000000160 ) ) ;
#8395 = PLANE ( 'NONE',  #6773 ) ;
#8396 = CARTESIAN_POINT ( 'NONE',  ( 0.000000000000000000, 0.000000000000000000, 205.0000000000000284 ) ) ;
#8397 =( NAMED_UNIT ( * ) SI_UNIT ( $, .STERADIAN. ) SOLID_ANGLE_UNIT ( ) );
#8398 = VECTOR ( 'NONE', #8885, 1000.000000000000000 ) ;
#8399 = CARTESIAN_POINT ( 'NONE',  ( -4.175648173966055587, 2.207990556236529844, -3.469390959564062626 ) ) ;
#8400 = CONTEXT_DEPENDENT_SHAPE_REPRESENTATION ( #12985, #2079 ) ;
#8401 = CARTESIAN_POINT ( 'NONE',  ( 217.4999999999999147, -85.00000000000009948, 0.000000000000000000 ) ) ;
#8402 = ORIENTED_EDGE ( 'NONE', *, *, #11033, .T. ) ;
#8403 = CARTESIAN_POINT ( 'NONE',  ( 236.4999999999999432, -85.00000000000007105, 50.00000000000001421 ) ) ;
#8404 = ORIENTED_EDGE ( 'NONE', *, *, #2992, .F. ) ;
#8405 = DIRECTION ( 'NONE',  ( 0.000000000000000000, 0.000000000000000000, 1.000000000000000000 ) ) ;
#8406 = CYLINDRICAL_SURFACE ( 'NONE', #2614, 2.500000000000000000 ) ;
#8407 = ORIENTED_EDGE ( 'NONE', *, *, #6453, .F. ) ;
#8408 = FACE_OUTER_BOUND ( 'NONE', #12726, .T. ) ;
#8409 = ORIENTED_EDGE ( 'NONE', *, *, #11917, .F. ) ;
#8410 = LINE ( 'NONE', #2550, #1988 ) ;
#8411 = DIRECTION ( 'NONE',  ( 0.000000000000000000, 0.000000000000000000, 1.000000000000000000 ) ) ;
#8412 = EDGE_LOOP ( 'NONE', ( #837, #3606, #8282 ) ) ;
#8413 = CYLINDRICAL_SURFACE ( 'NONE', #9900, 5.500000000000005329 ) ;
#8414 = DIRECTION ( 'NONE',  ( 0.000000000000000000, 0.000000000000000000, -1.000000000000000000 ) ) ;
#8415 = DIRECTION ( 'NONE',  ( -1.000000000000000000, -0.000000000000000000, -0.000000000000000000 ) ) ;
#8416 = EDGE_CURVE ( 'NONE', #6238, #2872, #12698, .T. ) ;
#8417 = ITEM_DEFINED_TRANSFORMATION ( 'NONE', 'NONE', #13945,  #14039 ) ;
#8418 = DIRECTION ( 'NONE',  ( 0.000000000000000000, 0.000000000000000000, 1.000000000000000000 ) ) ;
#8419 = EDGE_CURVE ( 'NONE', #8392, #2019, #13856, .T. ) ;
#8420 = EDGE_LOOP ( 'NONE', ( #12418, #1533, #1228, #3181 ) ) ;
#8421 = EDGE_LOOP ( 'NONE', ( #13868, #10246, #744, #7123 ) ) ;
#8422 = EDGE_LOOP ( 'NONE', ( #6890, #10633, #11320, #2722, #3898, #5433, #1619 ) ) ;
#8423 = ORIENTED_EDGE ( 'NONE', *, *, #13739, .T. ) ;
#8424 = FACE_OUTER_BOUND ( 'NONE', #3375, .T. ) ;
#8425 = ORIENTED_EDGE ( 'NONE', *, *, #7073, .F. ) ;
#8426 = LINE ( 'NONE', #12854, #9901 ) ;
#8427 = ORIENTED_EDGE ( 'NONE', *, *, #2929, .F. ) ;
#8428 = DIRECTION ( 'NONE',  ( -1.000000000000000000, -0.000000000000000000, -0.000000000000000000 ) ) ;
#8429 = ADVANCED_FACE ( 'NONE', ( #11686, #409, #4880, #14137, #2177 ), #4144, .F. ) ;
#8430 = DIRECTION ( 'NONE',  ( -1.000000000000000000, -0.000000000000000000, -0.000000000000000000 ) ) ;
#8431 = DIRECTION ( 'NONE',  ( -0.000000000000000000, -0.000000000000000000, 1.000000000000000000 ) ) ;
#8432 = FACE_OUTER_BOUND ( 'NONE', #10162, .T. ) ;
#8433 = CARTESIAN_POINT ( 'NONE',  ( -5.000000000000000888, -8.660254037844389075, 200.0000000000000000 ) ) ;
#8434 = EDGE_CURVE ( 'NONE', #9602, #11786, #2504, .T. ) ;
#8435 = EDGE_CURVE ( 'NONE', #3125, #13571, #9910, .T. ) ;
#8436 = DIRECTION ( 'NONE',  ( -0.000000000000000000, 0.000000000000000000, 1.000000000000000000 ) ) ;
#8437 = ORIENTED_EDGE ( 'NONE', *, *, #5281, .F. ) ;
#8438 = ORIENTED_EDGE ( 'NONE', *, *, #10705, .T. ) ;
#8439 = ADVANCED_FACE ( 'NONE', ( #7609 ), #1548, .T. ) ;
#8440 = LINE ( 'NONE', #5336, #969 ) ;
#8441 =( REPRESENTATION_RELATIONSHIP ('NONE','NONE', #11251, #11637 ) REPRESENTATION_RELATIONSHIP_WITH_TRANSFORMATION ( #2182 )SHAPE_REPRESENTATION_RELATIONSHIP( ) );
#8442 = DIRECTION ( 'NONE',  ( 1.000000000000000000, 0.000000000000000000, 0.000000000000000000 ) ) ;
#8443 = FACE_OUTER_BOUND ( 'NONE', #2260, .T. ) ;
#8444 = EDGE_CURVE ( 'NONE', #8392, #2665, #6439, .T. ) ;
#8445 = EDGE_CURVE ( 'NONE', #2036, #11751, #6462, .T. ) ;
#8446 = DIRECTION ( 'NONE',  ( -0.000000000000000000, -0.000000000000000000, 1.000000000000000000 ) ) ;
#8447 = EDGE_LOOP ( 'NONE', ( #12356, #4513, #11568, #10836 ) ) ;
#8448 = EDGE_CURVE ( 'NONE', #3716, #4493, #4218, .T. ) ;
#8449 = EDGE_CURVE ( 'NONE', #4728, #8297, #12221, .T. ) ;
#8450 = FACE_OUTER_BOUND ( 'NONE', #8774, .T. ) ;
#8451 = EDGE_CURVE ( 'NONE', #10393, #13274, #2731, .T. ) ;
#8452 = DIRECTION ( 'NONE',  ( -1.000000000000000000, -0.000000000000000000, -0.000000000000000000 ) ) ;
#8453 = DIRECTION ( 'NONE',  ( -1.000000000000000000, -6.123233995736766036E-17, -6.123233995736764803E-17 ) ) ;
#8454 = DIRECTION ( 'NONE',  ( -0.000000000000000000, -0.000000000000000000, -1.000000000000000000 ) ) ;
#8455 = ORIENTED_EDGE ( 'NONE', *, *, #11116, .F. ) ;
#8456 = VERTEX_POINT ( 'NONE', #10892 ) ;
#8457 = CYLINDRICAL_SURFACE ( 'NONE', #431, 2.100000000000000089 ) ;
#8458 = DIRECTION ( 'NONE',  ( 1.000000000000000000, 0.000000000000000000, 0.000000000000000000 ) ) ;
#8459 = ORIENTED_EDGE ( 'NONE', *, *, #1321, .F. ) ;
#8460 = LINE ( 'NONE', #9783, #10116 ) ;
#8461 = CIRCLE ( 'NONE', #4309, 2.500000000000002220 ) ;
#8462 =( LENGTH_UNIT ( ) NAMED_UNIT ( * ) SI_UNIT ( .MILLI., .METRE. ) );
#8463 = CYLINDRICAL_SURFACE ( 'NONE', #11536, 2.500000000000002220 ) ;
#8464 = CARTESIAN_POINT ( 'NONE',  ( -6.473970235329672780E-16, -4.862606272033106691, -3.745885042887442395 ) ) ;
#8465 = DIRECTION ( 'NONE',  ( 0.000000000000000000, 0.000000000000000000, -1.000000000000000000 ) ) ;
#8466 = PRESENTATION_STYLE_ASSIGNMENT (( #7385 ) ) ;
#8467 = CARTESIAN_POINT ( 'NONE',  ( 0.3226060873438401089, 2.189154565102731098, 0.5149999999999992362 ) ) ;
#8468 = CONTEXT_DEPENDENT_SHAPE_REPRESENTATION ( #10771, #3926 ) ;
#8469 = ADVANCED_FACE ( 'NONE', ( #5236 ), #5060, .T. ) ;
#8470 = EDGE_LOOP ( 'NONE', ( #12624, #12127, #12912, #2797 ) ) ;
#8471 = DIRECTION ( 'NONE',  ( 0.000000000000000000, 0.000000000000000000, -1.000000000000000000 ) ) ;
#8472 = AXIS2_PLACEMENT_3D ( 'NONE', #848, #5438, #6529 ) ;
#8473 = MANIFOLD_SOLID_BREP ( 'M5 Clearance Hole2', #3810 ) ;
#8474 = ORIENTED_EDGE ( 'NONE', *, *, #1880, .F. ) ;
#8475 = DIRECTION ( 'NONE',  ( -1.000000000000000000, 1.224646799147352714E-16, 0.000000000000000000 ) ) ;
#8476 = CARTESIAN_POINT ( 'NONE',  ( 134.9999999999999432, -56.99999999999997158, -169.9999999999999716 ) ) ;
#8477 = ORIENTED_EDGE ( 'NONE', *, *, #3174, .F. ) ;
#8478 = DIRECTION ( 'NONE',  ( -2.775557561562892929E-15, 1.000000000000000000, 0.000000000000000000 ) ) ;
#8479 = ORIENTED_EDGE ( 'NONE', *, *, #12585, .F. ) ;
#8480 = FACE_OUTER_BOUND ( 'NONE', #5144, .T. ) ;
#8481 = DIRECTION ( 'NONE',  ( 0.000000000000000000, 0.000000000000000000, 1.000000000000000000 ) ) ;
#8482 = VERTEX_POINT ( 'NONE', #3210 ) ;
#8483 = CIRCLE ( 'NONE', #4785, 5.000000000000004441 ) ;
#8484 = DIRECTION ( 'NONE',  ( -1.000000000000000000, -0.000000000000000000, -0.000000000000000000 ) ) ;
#8485 = CARTESIAN_POINT ( 'NONE',  ( 4.999999999999999112, 8.660254037844390851, 199.9990000000000236 ) ) ;
#8486 = VECTOR ( 'NONE', #10699, 1000.000000000000000 ) ;
#8487 = SHAPE_REPRESENTATION_RELATIONSHIP ( 'NONE' , 'NONE' ,  #10713, #13031 ) ;
#8488 = PLANE ( 'NONE',  #7866 ) ;
#8489 = ITEM_DEFINED_TRANSFORMATION ( 'NONE', 'NONE', #2367,  #14039 ) ;
#8490 = AXIS2_PLACEMENT_3D ( 'NONE', #13165, #11209, #9020 ) ;
#8491 = CARTESIAN_POINT ( 'NONE',  ( 0.000000000000000000, 0.000000000000000000, 0.000000000000000000 ) ) ;
#8492 = ADVANCED_FACE ( 'NONE', ( #9733 ), #8639, .F. ) ;
#8493 = ORIENTED_EDGE ( 'NONE', *, *, #6292, .F. ) ;
#8494 = ORIENTED_EDGE ( 'NONE', *, *, #4898, .F. ) ;
#8495 = VERTEX_POINT ( 'NONE', #9806 ) ;
#8496 = CIRCLE ( 'NONE', #13123, 2.041999999999999815 ) ;
#8497 = ORIENTED_EDGE ( 'NONE', *, *, #6688, .T. ) ;
#8498 = DIRECTION ( 'NONE',  ( -0.000000000000000000, -0.000000000000000000, 1.000000000000000000 ) ) ;
#8499 = ORIENTED_EDGE ( 'NONE', *, *, #3300, .F. ) ;
#8500 = CIRCLE ( 'NONE', #2248, 2.649999999999985700 ) ;
#8501 = ORIENTED_EDGE ( 'NONE', *, *, #13950, .T. ) ;
#8502 = DIRECTION ( 'NONE',  ( -0.000000000000000000, 1.000000000000000000, -0.000000000000000000 ) ) ;
#8503 = ORIENTED_EDGE ( 'NONE', *, *, #4388, .F. ) ;
#8504 = EDGE_CURVE ( 'NONE', #682, #13286, #13155, .T. ) ;
#8505 = CARTESIAN_POINT ( 'NONE',  ( 3.016506661494197328, 8.581769150706125103E-33, -7.007546303702493782E-17 ) ) ;
#8506 = VECTOR ( 'NONE', #3436, 1000.000000000000000 ) ;
#8507 = UNCERTAINTY_MEASURE_WITH_UNIT (LENGTH_MEASURE( 1.000000000000000082E-05 ), #6830, 'distance_accuracy_value', 'NONE');
#8508 = AXIS2_PLACEMENT_3D ( 'NONE', #10842, #2932, #1832 ) ;
#8509 = DIRECTION ( 'NONE',  ( 0.000000000000000000, 0.000000000000000000, 1.000000000000000000 ) ) ;
#8510 = CARTESIAN_POINT ( 'NONE',  ( 2.804994570502171047, 3.229033611042449792, -3.526374918436834704 ) ) ;
#8511 = AXIS2_PLACEMENT_3D ( 'NONE', #6905, #11338, #5819 ) ;
#8512 = DIRECTION ( 'NONE',  ( 1.000000000000000000, 0.000000000000000000, 0.000000000000000000 ) ) ;
#8513 = TOROIDAL_SURFACE ( 'NONE', #9687, 10.20000000000000107, 0.2000000000000031197 ) ;
#8514 = CARTESIAN_POINT ( 'NONE',  ( 21.00000000000000355, 2.789133085058097101E-16, -2.055000000000000160 ) ) ;
#8515 = EDGE_LOOP ( 'NONE', ( #6627, #12671 ) ) ;
#8516 = VECTOR ( 'NONE', #5771, 1000.000000000000000 ) ;
#8517 = EDGE_LOOP ( 'NONE', ( #10174, #7608 ) ) ;
#8518 = AXIS2_PLACEMENT_3D ( 'NONE', #6388, #14209, #9942 ) ;
#8519 = B_SPLINE_CURVE_WITH_KNOTS ( 'NONE', 3,
 ( #5004, #4055, #2977, #2898, #13838, #3912, #2827, #7245 ),
 .UNSPECIFIED., .F., .F.,
 ( 4, 2, 2, 4 ),
 ( 0.005725059856848645212, 0.006314084072593634418, 0.006903108288338624492, 0.008081156719828603771 ),
 .UNSPECIFIED. ) ;
#8520 = CARTESIAN_POINT ( 'NONE',  ( 305.0000000000000000, -36.99999999999997868, -181.5021515430661054 ) ) ;
#8521 = CARTESIAN_POINT ( 'NONE',  ( -299.9999999999999432, -95.00000000000008527, 30.00000000000002842 ) ) ;
#8522 = ADVANCED_FACE ( 'NONE', ( #7953 ), #8513, .T. ) ;
#8523 = DIRECTION ( 'NONE',  ( 0.000000000000000000, 1.000000000000000000, 0.000000000000000000 ) ) ;
#8524 = VECTOR ( 'NONE', #13183, 1000.000000000000000 ) ;
#8525 = CARTESIAN_POINT ( 'NONE',  ( 304.9999999999999432, 45.00000000000001421, 0.000000000000000000 ) ) ;
#8526 = EDGE_LOOP ( 'NONE', ( #11898, #10981, #13665, #10084, #9045, #7544, #11205, #39 ) ) ;
#8527 = COLOUR_RGB ( '',0.8941176470588234615, 0.8941176470588234615, 0.8941176470588234615 ) ;
#8528 = CARTESIAN_POINT ( 'NONE',  ( 2.740000000000000213, 0.5150000000000035660, -0.9838866223905657904 ) ) ;
#8529 = CARTESIAN_POINT ( 'NONE',  ( 4.999999999999997335, 5.204748896376250699E-16, -4.250000000000000000 ) ) ;
#8530 = DIRECTION ( 'NONE',  ( 6.123233995736766036E-17, 0.000000000000000000, -1.000000000000000000 ) ) ;
#8531 = CARTESIAN_POINT ( 'NONE',  ( -30.00000000000002842, -15.00000000000000000, 200.0000000000000000 ) ) ;
#8532 = EDGE_CURVE ( 'NONE', #4042, #7902, #4502, .T. ) ;
#8533 = ADVANCED_FACE ( 'NONE', ( #6878 ), #5583, .F. ) ;
#8534 = ORIENTED_EDGE ( 'NONE', *, *, #3563, .T. ) ;
#8535 =( REPRESENTATION_RELATIONSHIP ('NONE','NONE', #11251, #5332 ) REPRESENTATION_RELATIONSHIP_WITH_TRANSFORMATION ( #13277 )SHAPE_REPRESENTATION_RELATIONSHIP( ) );
#8536 = ADVANCED_FACE ( 'NONE', ( #5718 ), #12006, .F. ) ;
#8537 = EDGE_LOOP ( 'NONE', ( #7810, #11478, #11643 ) ) ;
#8538 = FACE_OUTER_BOUND ( 'NONE', #4891, .T. ) ;
#8539 = AXIS2_PLACEMENT_3D ( 'NONE', #11785, #12644, #5049 ) ;
#8540 = LINE ( 'NONE', #7592, #11375 ) ;
#8541 = PRODUCT_DEFINITION_CONTEXT ( 'detailed design', #12764, 'design' ) ;
#8542 = ORIENTED_EDGE ( 'NONE', *, *, #1431, .T. ) ;
#8543 = DIRECTION ( 'NONE',  ( -1.000000000000000000, 1.110223024625157487E-14, 0.000000000000000000 ) ) ;
#8544 = AXIS2_PLACEMENT_3D ( 'NONE', #12136, #8730, #13151 ) ;
#8545 = CARTESIAN_POINT ( 'NONE',  ( 4.204115023516791005, -1.660442669500199919, -3.602151381774560068 ) ) ;
#8546 = DIRECTION ( 'NONE',  ( -0.000000000000000000, 1.000000000000000000, -0.000000000000000000 ) ) ;
#8547 = SURFACE_STYLE_USAGE ( .BOTH. , #2976 ) ;
#8548 = AXIS2_PLACEMENT_3D ( 'NONE', #10664, #9497, #545 ) ;
#8549 = ITEM_DEFINED_TRANSFORMATION ( 'NONE', 'NONE', #11645,  #14039 ) ;
#8550 = VERTEX_POINT ( 'NONE', #10014 ) ;
#8551 = DIRECTION ( 'NONE',  ( -1.000000000000000000, 0.000000000000000000, 0.000000000000000000 ) ) ;
#8552 = ORIENTED_EDGE ( 'NONE', *, *, #2242, .F. ) ;
#8553 = DIRECTION ( 'NONE',  ( -0.000000000000000000, -0.000000000000000000, -1.000000000000000000 ) ) ;
#8554 = DIRECTION ( 'NONE',  ( -0.000000000000000000, 0.000000000000000000, 1.000000000000000000 ) ) ;
#8555 = VERTEX_POINT ( 'NONE', #182 ) ;
#8556 = LINE ( 'NONE', #10601, #4122 ) ;
#8557 = ORIENTED_EDGE ( 'NONE', *, *, #12273, .T. ) ;
#8558 = VECTOR ( 'NONE', #9261, 1000.000000000000000 ) ;
#8559 = CARTESIAN_POINT ( 'NONE',  ( 299.9999999999999432, -95.00000000000008527, -186.2999999999999829 ) ) ;
#8560 = PRODUCT_DEFINITION_SHAPE ( 'NONE', 'NONE',  #14380 ) ;
#8561 = DIRECTION ( 'NONE',  ( -1.000000000000000000, -0.000000000000000000, -0.000000000000000000 ) ) ;
#8562 = ORIENTED_EDGE ( 'NONE', *, *, #10342, .T. ) ;
#8563 = CARTESIAN_POINT ( 'NONE',  ( 140.0000000000000000, -75.00000000000008527, -186.2999999999999829 ) ) ;
#8564 = EDGE_CURVE ( 'NONE', #8653, #191, #4816, .T. ) ;
#8565 = VECTOR ( 'NONE', #7153, 1000.000000000000000 ) ;
#8566 = DIRECTION ( 'NONE',  ( -1.000000000000000000, -0.000000000000000000, -0.000000000000000000 ) ) ;
#8567 = CARTESIAN_POINT ( 'NONE',  ( 303.3333333333333144, -25.00000000000000000, 222.5000000000000853 ) ) ;
#8568 = ORIENTED_EDGE ( 'NONE', *, *, #1431, .F. ) ;
#8569 = AXIS2_PLACEMENT_3D ( 'NONE', #3176, #1031, #3388 ) ;
#8570 = ORIENTED_EDGE ( 'NONE', *, *, #4642, .F. ) ;
#8571 = CARTESIAN_POINT ( 'NONE',  ( -124.9999999999999432, -65.00000000000008527, 40.00000000000000000 ) ) ;
#8572 = ORIENTED_EDGE ( 'NONE', *, *, #11185, .T. ) ;
#8573 = CIRCLE ( 'NONE', #13431, 2.041999999999999815 ) ;
#8574 = DIRECTION ( 'NONE',  ( 1.000000000000000000, 0.000000000000000000, 0.000000000000000000 ) ) ;
#8575 = UNCERTAINTY_MEASURE_WITH_UNIT (LENGTH_MEASURE( 1.000000000000000082E-05 ), #1091, 'distance_accuracy_value', 'NONE');
#8576 = ORIENTED_EDGE ( 'NONE', *, *, #6222, .F. ) ;
#8577 = VECTOR ( 'NONE', #5178, 1000.000000000000000 ) ;
#8578 = ORIENTED_EDGE ( 'NONE', *, *, #6768, .F. ) ;
#8579 = CARTESIAN_POINT ( 'NONE',  ( 136.6666666666666288, -25.00000000000000000, 222.5000000000000853 ) ) ;
#8580 = EDGE_LOOP ( 'NONE', ( #5729, #2845 ) ) ;
#8581 = FACE_OUTER_BOUND ( 'NONE', #12215, .T. ) ;
#8582 = DIRECTION ( 'NONE',  ( 0.000000000000000000, 0.000000000000000000, -1.000000000000000000 ) ) ;
#8583 = CARTESIAN_POINT ( 'NONE',  ( 144.9999999999999716, -64.99999999999997158, 10.00000000000000000 ) ) ;
#8584 = ADVANCED_FACE ( 'NONE', ( #10076 ), #5734, .F. ) ;
#8585 = AXIS2_PLACEMENT_3D ( 'NONE', #4994, #2816, #1712 ) ;
#8586 = CARTESIAN_POINT ( 'NONE',  ( 2.500000000000000000, -2.357898499370432166, 3.035766082959412415E-15 ) ) ;
#8587 = CARTESIAN_POINT ( 'NONE',  ( 142.6500000000000057, -95.00000000000008527, -169.9999999999999716 ) ) ;
#8588 = ORIENTED_EDGE ( 'NONE', *, *, #1391, .T. ) ;
#8589 = AXIS2_PLACEMENT_3D ( 'NONE', #12392, #1358, #11523 ) ;
#8590 = EDGE_CURVE ( 'NONE', #12690, #145, #3207, .T. ) ;
#8591 = EDGE_LOOP ( 'NONE', ( #5532, #2801, #1781, #10552 ) ) ;
#8592 = CARTESIAN_POINT ( 'NONE',  ( -30.00000000000002842, -225.0000000000000000, 169.9999999999999716 ) ) ;
#8593 = CIRCLE ( 'NONE', #10443, 7.983406227920510467 ) ;
#8594 = ORIENTED_EDGE ( 'NONE', *, *, #2946, .T. ) ;
#8595 = CARTESIAN_POINT ( 'NONE',  ( 137.6499999999999488, -56.99999999999997158, 10.00000000000000178 ) ) ;
#8596 = CARTESIAN_POINT ( 'NONE',  ( 0.06760930072668806801, -4.837354856632045452E-15, 0.000000000000000000 ) ) ;
#8597 = DIRECTION ( 'NONE',  ( -0.000000000000000000, -0.000000000000000000, 1.000000000000000000 ) ) ;
#8598 = ORIENTED_EDGE ( 'NONE', *, *, #1761, .F. ) ;
#8599 = CIRCLE ( 'NONE', #11370, 2.500000000000002220 ) ;
#8600 = PLANE ( 'NONE',  #3052 ) ;
#8601 = DIRECTION ( 'NONE',  ( 0.000000000000000000, 0.000000000000000000, -1.000000000000000000 ) ) ;
#8602 = DIRECTION ( 'NONE',  ( 0.000000000000000000, 0.000000000000000000, -1.000000000000000000 ) ) ;
#8603 = AXIS2_PLACEMENT_3D ( 'NONE', #13522, #5916, #4764 ) ;
#8604 = FACE_OUTER_BOUND ( 'NONE', #9819, .T. ) ;
#8605 = EDGE_CURVE ( 'NONE', #5737, #10602, #11303, .T. ) ;
#8606 = VERTEX_POINT ( 'NONE', #2532 ) ;
#8607 = EDGE_CURVE ( 'NONE', #11069, #2351, #1079, .T. ) ;
#8608 = EDGE_LOOP ( 'NONE', ( #13112, #13612, #10066, #2999 ) ) ;
#8609 = DIRECTION ( 'NONE',  ( 0.000000000000000000, 0.8660254037844380415, -0.5000000000000011102 ) ) ;
#8610 = CARTESIAN_POINT ( 'NONE',  ( 2.500000000000000000, 2.357898499370433054, -1.951563910473907981E-15 ) ) ;
#8612 = VERTEX_POINT ( 'NONE', #8850 ) ;
#8611 = TOROIDAL_SURFACE ( 'NONE', #10467, 2.700000000000000622, 0.2000000000000000111 ) ;
#8613 = CARTESIAN_POINT ( 'NONE',  ( 303.3333333333333144, -14.99999999999999822, 222.5000000000000853 ) ) ;
#8614 = ADVANCED_FACE ( 'NONE', ( #1356 ), #13473, .F. ) ;
#8615 = AXIS2_PLACEMENT_3D ( 'NONE', #12102, #2228, #5429 ) ;
#8616 = DIRECTION ( 'NONE',  ( 1.000000000000000000, 0.000000000000000000, 0.000000000000000000 ) ) ;
#8617 = DIRECTION ( 'NONE',  ( -0.000000000000000000, -0.000000000000000000, 1.000000000000000000 ) ) ;
#8618 = SURFACE_SIDE_STYLE ('',( #1719 ) ) ;
#8619 = EDGE_CURVE ( 'NONE', #2208, #2542, #8030, .T. ) ;
#8620 = ITEM_DEFINED_TRANSFORMATION ( 'NONE', 'NONE', #3535,  #14039 ) ;
#8621 = CIRCLE ( 'NONE', #5618, 10.00000000000000000 ) ;
#8622 = VERTEX_POINT ( 'NONE', #3616 ) ;
#8623 = CARTESIAN_POINT ( 'NONE',  ( 197.5000000000000000, -90.00000000000007105, 50.00000000000001421 ) ) ;
#8624 = AXIS2_PLACEMENT_3D ( 'NONE', #9624, #11726, #13816 ) ;
#8625 = PRESENTATION_LAYER_ASSIGNMENT (  '', '', ( #7463 ) ) ;
#8626 = EDGE_LOOP ( 'NONE', ( #1999, #12646 ) ) ;
#8627 = AXIS2_PLACEMENT_3D ( 'NONE', #4374, #7548, #8719 ) ;
#8628 = FACE_OUTER_BOUND ( 'NONE', #5941, .T. ) ;
#8629 = DIRECTION ( 'NONE',  ( 0.000000000000000000, 0.000000000000000000, -1.000000000000000000 ) ) ;
#8630 = ORIENTED_EDGE ( 'NONE', *, *, #10119, .F. ) ;
#8631 = CARTESIAN_POINT ( 'NONE',  ( 0.000000000000000000, -0.5149999999999909095, -2.349999999999999201 ) ) ;
#8632 = ORIENTED_EDGE ( 'NONE', *, *, #11466, .F. ) ;
#8633 = CARTESIAN_POINT ( 'NONE',  ( 211.3397459621556038, -80.00000000000007105, 170.0000000000000000 ) ) ;
#8634 = EDGE_CURVE ( 'NONE', #10653, #13016, #5515, .T. ) ;
#8635 = DIRECTION ( 'NONE',  ( 0.000000000000000000, 0.000000000000000000, 1.000000000000000000 ) ) ;
#8638 = EDGE_LOOP ( 'NONE', ( #9052, #1313, #6802, #5524 ) ) ;
#8637 = CIRCLE ( 'NONE', #4707, 2.649999999999985700 ) ;
#8636 = AXIS2_PLACEMENT_3D ( 'NONE', #9761, #10781, #7358 ) ;
#8639 = PLANE ( 'NONE',  #7351 ) ;
#8640 = EDGE_CURVE ( 'NONE', #8550, #11373, #2966, .T. ) ;
#8641 = CARTESIAN_POINT ( 'NONE',  ( 132.4999999999999716, 45.00000000000001421, 0.000000000000000000 ) ) ;
#8642 = PRODUCT_DEFINITION_FORMATION_WITH_SPECIFIED_SOURCE ( 'ANY', '', #4495, .NOT_KNOWN. ) ;
#8643 = MECHANICAL_DESIGN_GEOMETRIC_PRESENTATION_REPRESENTATION (  '', ( #13038 ), #4211 ) ;
#8644 = DIRECTION ( 'NONE',  ( 1.000000000000000000, 0.000000000000000000, 0.000000000000000000 ) ) ;
#8645 = EDGE_CURVE ( 'NONE', #10577, #5028, #2262, .T. ) ;
#8646 = DIRECTION ( 'NONE',  ( -0.000000000000000000, 0.000000000000000000, -1.000000000000000000 ) ) ;
#8647 = VERTEX_POINT ( 'NONE', #4718 ) ;
#8648 = EDGE_LOOP ( 'NONE', ( #11208, #9016, #2029, #2875 ) ) ;
#8649 = DIRECTION ( 'NONE',  ( 1.000000000000000000, 0.000000000000000000, 0.000000000000000000 ) ) ;
#8650 = AXIS2_PLACEMENT_3D ( 'NONE', #10597, #8405, #1654 ) ;
#8651 = ORIENTED_EDGE ( 'NONE', *, *, #167, .F. ) ;
#8652 = CARTESIAN_POINT ( 'NONE',  ( -4.000000000000000000, 2.309401076758498483, -3.433295621305379353 ) ) ;
#8653 = VERTEX_POINT ( 'NONE', #13536 ) ;
#8654 = ORIENTED_EDGE ( 'NONE', *, *, #11473, .T. ) ;
#8655 = DIRECTION ( 'NONE',  ( 0.000000000000000000, 0.000000000000000000, -1.000000000000000000 ) ) ;
#8656 = EDGE_LOOP ( 'NONE', ( #11795, #1974, #2348, #5287, #594 ) ) ;
#8657 = DIRECTION ( 'NONE',  ( 0.000000000000000000, 0.000000000000000000, 1.000000000000000000 ) ) ;
#8658 = CARTESIAN_POINT ( 'NONE',  ( 469.9999999999998863, -25.00000000000000000, -190.0000000000000000 ) ) ;
#8659 = MANIFOLD_SOLID_BREP ( 'Hex', #12157 ) ;
#8660 = CARTESIAN_POINT ( 'NONE',  ( 0.000000000000000000, 2.349999999999998312, -0.5150000000000000133 ) ) ;
#8661 = CARTESIAN_POINT ( 'NONE',  ( 2.500000000000000000, -2.357898499370432610, 3.252606517456513302E-15 ) ) ;
#8662 = ORIENTED_EDGE ( 'NONE', *, *, #8532, .F. ) ;
#8663 = VERTEX_POINT ( 'NONE', #11447 ) ;
#8664 = ADVANCED_FACE ( 'NONE', ( #2669 ), #6641, .F. ) ;
#8665 = CARTESIAN_POINT ( 'NONE',  ( -5.000000000000000888, 8.660254037844390851, 210.0000000000000000 ) ) ;
#8666 = VECTOR ( 'NONE', #4219, 1000.000000000000000 ) ;
#8667 = EDGE_LOOP ( 'NONE', ( #11530, #1951, #4428, #7743 ) ) ;
#8668 = DIRECTION ( 'NONE',  ( 0.000000000000000000, 0.000000000000000000, -1.000000000000000000 ) ) ;
#8669 = DIRECTION ( 'NONE',  ( -0.000000000000000000, 0.000000000000000000, 1.000000000000000000 ) ) ;
#8670 = FACE_BOUND ( 'NONE', #6148, .T. ) ;
#8671 = EDGE_LOOP ( 'NONE', ( #9577, #4697 ) ) ;
#8672 = PLANE ( 'NONE',  #9301 ) ;
#8673 = B_SPLINE_CURVE_WITH_KNOTS ( 'NONE', 3,
 ( #10933, #3389, #9986, #890, #4186, #4480 ),
 .UNSPECIFIED., .F., .F.,
 ( 4, 2, 4 ),
 ( -3.640115492409406142E-06, 0.0002066546034003385283, 0.0004169493222930864334 ),
 .UNSPECIFIED. ) ;
#8674 = CARTESIAN_POINT ( 'NONE',  ( -217.3499999999999375, -85.00000000000009948, 40.00000000000000000 ) ) ;
#8675 = DIRECTION ( 'NONE',  ( 1.000000000000000000, 0.000000000000000000, -6.123233995736766036E-17 ) ) ;
#8676 = DIRECTION ( 'NONE',  ( 1.000000000000000000, 0.000000000000000000, 0.000000000000000000 ) ) ;
#8677 = ORIENTED_EDGE ( 'NONE', *, *, #9958, .F. ) ;
#8678 = EDGE_CURVE ( 'NONE', #6402, #2854, #5939, .T. ) ;
#8679 = VERTEX_POINT ( 'NONE', #3691 ) ;
#8680 = DIRECTION ( 'NONE',  ( 1.000000000000000000, 0.000000000000000000, 0.000000000000000000 ) ) ;
#8681 = PRODUCT_DEFINITION_SHAPE ( 'NONE', 'NONE',  #14340 ) ;
#8682 = DIRECTION ( 'NONE',  ( 1.000000000000000000, 0.000000000000000000, 0.000000000000000000 ) ) ;
#8683 = ORIENTED_EDGE ( 'NONE', *, *, #7093, .F. ) ;
#8685 = EDGE_CURVE ( 'NONE', #5289, #13737, #7160, .T. ) ;
#8684 = FACE_OUTER_BOUND ( 'NONE', #9615, .T. ) ;
#8686 = EDGE_CURVE ( 'NONE', #8193, #13622, #13615, .T. ) ;
#8687 = PLANE ( 'NONE',  #5266 ) ;
#8688 = DIRECTION ( 'NONE',  ( -1.000000000000000000, 0.000000000000000000, 0.000000000000000000 ) ) ;
#8689 = CARTESIAN_POINT ( 'NONE',  ( 88.00000000000000000, 0.000000000000000000, -188.0000000000000000 ) ) ;
#8690 = VECTOR ( 'NONE', #9212, 1000.000000000000114 ) ;
#8691 = VECTOR ( 'NONE', #6791, 1000.000000000000000 ) ;
#8692 = ORIENTED_EDGE ( 'NONE', *, *, #7820, .T. ) ;
#8693 = CARTESIAN_POINT ( 'NONE',  ( 217.9449999999999079, -85.00000000000009948, -18.00000000000000355 ) ) ;
#8694 = ORIENTED_EDGE ( 'NONE', *, *, #4375, .T. ) ;
#8695 = CARTESIAN_POINT ( 'NONE',  ( -304.9999999999999432, -75.00000000000008527, 30.00000000000002842 ) ) ;
#8696 = CYLINDRICAL_SURFACE ( 'NONE', #1615, 12.44999999999999929 ) ;
#8697 = AXIS2_PLACEMENT_3D ( 'NONE', #12483, #6618, #11052 ) ;
#8698 = EDGE_LOOP ( 'NONE', ( #1577, #9035, #3110, #2115 ) ) ;
#8699 = ORIENTED_EDGE ( 'NONE', *, *, #5529, .F. ) ;
#8701 = EDGE_CURVE ( 'NONE', #246, #9196, #9353, .T. ) ;
#8700 = PLANE ( 'NONE',  #3851 ) ;
#8702 = EDGE_CURVE ( 'NONE', #7268, #5823, #5864, .T. ) ;
#8703 = PLANE ( 'NONE',  #9209 ) ;
#8704 = ORIENTED_EDGE ( 'NONE', *, *, #3623, .T. ) ;
#8705 = FILL_AREA_STYLE ('',( #916 ) ) ;
#8706 = PLANE ( 'NONE',  #10170 ) ;
#8707 = FACE_OUTER_BOUND ( 'NONE', #8797, .T. ) ;
#8708 =( NAMED_UNIT ( * ) PLANE_ANGLE_UNIT ( ) SI_UNIT ( $, .RADIAN. ) );
#8709 = CARTESIAN_POINT ( 'NONE',  ( 124.9999999999999858, 55.00000000000000711, 10.00000000000000000 ) ) ;
#8710 = CARTESIAN_POINT ( 'NONE',  ( -4.000000000000000000, -2.472261339043343220, -3.687027428081192326 ) ) ;
#8711 = VECTOR ( 'NONE', #1886, 1000.000000000000000 ) ;
#8712 = ORIENTED_EDGE ( 'NONE', *, *, #9714, .F. ) ;
#8713 = ORIENTED_EDGE ( 'NONE', *, *, #14180, .T. ) ;
#8714 = ADVANCED_FACE ( 'NONE', ( #9200 ), #1492, .T. ) ;
#8715 = EDGE_CURVE ( 'NONE', #13411, #5681, #2003, .T. ) ;
#8716 = DIRECTION ( 'NONE',  ( -0.000000000000000000, 0.000000000000000000, -1.000000000000000000 ) ) ;
#8717 = ORIENTED_EDGE ( 'NONE', *, *, #7570, .F. ) ;
#8718 = EDGE_CURVE ( 'NONE', #8809, #12847, #8250, .T. ) ;
#8719 = DIRECTION ( 'NONE',  ( 0.000000000000000000, 0.000000000000000000, -1.000000000000000000 ) ) ;
#8720 = VERTEX_POINT ( 'NONE', #8173 ) ;
#8721 = TOROIDAL_SURFACE ( 'NONE', #4091, 2.700000000000000622, 0.2000000000000000111 ) ;
#8722 = EDGE_LOOP ( 'NONE', ( #8503, #2912, #309, #4731, #7355 ) ) ;
#8723 = DIRECTION ( 'NONE',  ( -0.000000000000000000, -0.000000000000000000, -1.000000000000000000 ) ) ;
#8724 = ORIENTED_EDGE ( 'NONE', *, *, #1737, .T. ) ;
#8725 = DIRECTION ( 'NONE',  ( 1.000000000000000000, 0.000000000000000000, 0.000000000000000000 ) ) ;
#8726 = VECTOR ( 'NONE', #6241, 1000.000000000000000 ) ;
#8727 = DIRECTION ( 'NONE',  ( 1.000000000000000000, 0.000000000000000000, 0.000000000000000000 ) ) ;
#8728 = CARTESIAN_POINT ( 'NONE',  ( 119.9999999999999147, -24.99999999999999289, 19.99999999999998934 ) ) ;
#8729 = AXIS2_PLACEMENT_3D ( 'NONE', #11138, #5471, #2355 ) ;
#8730 = DIRECTION ( 'NONE',  ( -0.000000000000000000, -0.000000000000000000, 1.000000000000000000 ) ) ;
#8731 = FACE_OUTER_BOUND ( 'NONE', #5897, .T. ) ;
#8732 = CIRCLE ( 'NONE', #5487, 13.50000000000000000 ) ;
#8733 = ORIENTED_EDGE ( 'NONE', *, *, #3233, .F. ) ;
#8734 = AXIS2_PLACEMENT_3D ( 'NONE', #2807, #9259, #1409 ) ;
#8735 = EDGE_LOOP ( 'NONE', ( #13219, #10907, #2495, #7579 ) ) ;
#8736 = CIRCLE ( 'NONE', #5709, 12.44999999999999929 ) ;
#8738 = DIRECTION ( 'NONE',  ( 0.000000000000000000, -1.000000000000000000, 0.000000000000000000 ) ) ;
#8737 = VECTOR ( 'NONE', #13218, 1000.000000000000114 ) ;
#8739 = ORIENTED_EDGE ( 'NONE', *, *, #9631, .F. ) ;
#8740 = FACE_OUTER_BOUND ( 'NONE', #7311, .T. ) ;
#8741 = CARTESIAN_POINT ( 'NONE',  ( 1.393927851585479161, -4.043713361053543842, -3.526374918436840922 ) ) ;
#8742 = FACE_BOUND ( 'NONE', #5135, .T. ) ;
#8743 = AXIS2_PLACEMENT_3D ( 'NONE', #6107, #9593, #12702 ) ;
#8744 = VERTEX_POINT ( 'NONE', #1566 ) ;
#8745 = VECTOR ( 'NONE', #12070, 1000.000000000000000 ) ;
#8746 = CARTESIAN_POINT ( 'NONE',  ( 2.500000000000000000, -2.357898499370432610, 3.252606517456513302E-15 ) ) ;
#8747 = EDGE_CURVE ( 'NONE', #7034, #5388, #3829, .T. ) ;
#8748 = AXIS2_PLACEMENT_3D ( 'NONE', #2908, #11757, #1809 ) ;
#8749 = LINE ( 'NONE', #3323, #11349 ) ;
#8750 = DIRECTION ( 'NONE',  ( -6.123233995736766036E-17, 0.000000000000000000, -1.000000000000000000 ) ) ;
#8751 = AXIS2_PLACEMENT_3D ( 'NONE', #7818, #3277, #1212 ) ;
#8752 = PLANE ( 'NONE',  #2081 ) ;
#8753 = VERTEX_POINT ( 'NONE', #4997 ) ;
#8754 = CIRCLE ( 'NONE', #8042, 4.000000000000000000 ) ;
#8755 = VERTEX_POINT ( 'NONE', #10434 ) ;
#8756 = LINE ( 'NONE', #10940, #13214 ) ;
#8757 = DIRECTION ( 'NONE',  ( 1.000000000000000000, 0.000000000000000000, 0.000000000000000000 ) ) ;
#8758 = VECTOR ( 'NONE', #13302, 1000.000000000000000 ) ;
#8759 = VERTEX_POINT ( 'NONE', #2605 ) ;
#8760 = DIRECTION ( 'NONE',  ( 1.000000000000000000, 0.000000000000000000, -0.000000000000000000 ) ) ;
#8761 = CARTESIAN_POINT ( 'NONE',  ( 307.4999999999999432, 45.00000000000001421, 0.000000000000000000 ) ) ;
#8762 = LINE ( 'NONE', #6588, #1122 ) ;
#8763 = DIRECTION ( 'NONE',  ( 6.123233995736766036E-17, -1.000000000000000000, 0.000000000000000000 ) ) ;
#8764 = CIRCLE ( 'NONE', #6216, 4.250000000000000000 ) ;
#8765 = ORIENTED_EDGE ( 'NONE', *, *, #2122, .F. ) ;
#8766 = ADVANCED_FACE ( 'NONE', ( #13831 ), #7026, .F. ) ;
#8767 = CARTESIAN_POINT ( 'NONE',  ( 2.500000000000000000, -2.357898499370432610, 3.252606517456513302E-15 ) ) ;
#8768 = PRODUCT_DEFINITION_SHAPE ( 'NONE', 'NONE',  #14313 ) ;
#8769 = MANIFOLD_SOLID_BREP ( 'EndChamfer', #13764 ) ;
#8770 = ORIENTED_EDGE ( 'NONE', *, *, #11830, .T. ) ;
#8771 = DIRECTION ( 'NONE',  ( 0.000000000000000000, 1.000000000000000000, 0.000000000000000000 ) ) ;
#8772 = FACE_OUTER_BOUND ( 'NONE', #10904, .T. ) ;
#8773 = ORIENTED_EDGE ( 'NONE', *, *, #13158, .F. ) ;
#8774 = EDGE_LOOP ( 'NONE', ( #5235, #6873, #3945, #1369 ) ) ;
#8776 = VECTOR ( 'NONE', #5403, 1000.000000000000114 ) ;
#8775 = CARTESIAN_POINT ( 'NONE',  ( -5.000000000000000888, 8.660254037844390851, -210.0000000000000000 ) ) ;
#8777 = CARTESIAN_POINT ( 'NONE',  ( 0.000000000000000000, 0.000000000000000000, -250.0000000000000000 ) ) ;
#8778 = DIRECTION ( 'NONE',  ( -1.000000000000000000, 0.000000000000000000, 0.000000000000000000 ) ) ;
#8779 = CIRCLE ( 'NONE', #3683, 2.041999999999999815 ) ;
#8780 = CARTESIAN_POINT ( 'NONE',  ( 2.740000000000000213, 0.000000000000000000, 0.000000000000000000 ) ) ;
#8781 = CARTESIAN_POINT ( 'NONE',  ( 0.000000000000000000, -1.178949249685218748, -2.041999999999998039 ) ) ;
#8782 = CARTESIAN_POINT ( 'NONE',  ( 53.33333333333330017, -14.99999999999999822, 222.5000000000000853 ) ) ;
#8783 = CARTESIAN_POINT ( 'NONE',  ( 140.0000000000000000, -95.00000000000008527, -190.0000000000000000 ) ) ;
#8784 = ITEM_DEFINED_TRANSFORMATION ( 'NONE', 'NONE', #10719,  #14039 ) ;
#8785 = CARTESIAN_POINT ( 'NONE',  ( -4.000000000000000000, -1.680117682357936904, -3.316611593218794951 ) ) ;
#8786 = VERTEX_POINT ( 'NONE', #9785 ) ;
#8787 = ORIENTED_EDGE ( 'NONE', *, *, #12071, .T. ) ;
#8788 = ADVANCED_FACE ( 'NONE', ( #10357 ), #4130, .F. ) ;
#8789 = CYLINDRICAL_SURFACE ( 'NONE', #544, 2.649999999999985700 ) ;
#8790 =( REPRESENTATION_RELATIONSHIP ('NONE','NONE', #11251, #13104 ) REPRESENTATION_RELATIONSHIP_WITH_TRANSFORMATION ( #6466 )SHAPE_REPRESENTATION_RELATIONSHIP( ) );
#8791 = VERTEX_POINT ( 'NONE', #4198 ) ;
#8792 = DIRECTION ( 'NONE',  ( 1.110223024625157487E-14, 1.000000000000000000, 0.000000000000000000 ) ) ;
#8793 = AXIS2_PLACEMENT_3D ( 'NONE', #13677, #3747, #9183 ) ;
#8794 = ORIENTED_EDGE ( 'NONE', *, *, #3577, .T. ) ;
#8795 = EDGE_LOOP ( 'NONE', ( #6524, #4487, #8914, #12725 ) ) ;
#8796 = DIRECTION ( 'NONE',  ( 0.000000000000000000, 0.000000000000000000, 1.000000000000000000 ) ) ;
#8797 = EDGE_LOOP ( 'NONE', ( #11844, #3335, #6617, #7643 ) ) ;
#8798 = CARTESIAN_POINT ( 'NONE',  ( -4.197393957002303999, -7.773935952363655451E-14, -3.503767560748929810 ) ) ;
#8799 = CARTESIAN_POINT ( 'NONE',  ( -0.7826237921249277196, 0.000000000000000000, 0.000000000000000000 ) ) ;
#8800 = CARTESIAN_POINT ( 'NONE',  ( 1.794155980045909482, 0.000000000000000000, 0.000000000000000000 ) ) ;
#8801 = ADVANCED_FACE ( 'NONE', ( #13041 ), #1938, .F. ) ;
#8802 = ADVANCED_FACE ( 'NONE', ( #833 ), #6294, .F. ) ;
#8803 = LINE ( 'NONE', #3301, #8776 ) ;
#8804 =( NAMED_UNIT ( * ) SI_UNIT ( $, .STERADIAN. ) SOLID_ANGLE_UNIT ( ) );
#8805 = AXIS2_PLACEMENT_3D ( 'NONE', #1469, #9248, #9321 ) ;
#8806 = DIRECTION ( 'NONE',  ( -1.000000000000000000, -0.000000000000000000, -0.000000000000000000 ) ) ;
#8807 = VERTEX_POINT ( 'NONE', #2009 ) ;
#8808 = ADVANCED_FACE ( 'NONE', ( #9849 ), #8687, .F. ) ;
#8809 = VERTEX_POINT ( 'NONE', #687 ) ;
#8810 = AXIS2_PLACEMENT_3D ( 'NONE', #12413, #11407, #1519 ) ;
#8811 = LINE ( 'NONE', #6492, #8154 ) ;
#8812 = ORIENTED_EDGE ( 'NONE', *, *, #13832, .F. ) ;
#8813 = DIRECTION ( 'NONE',  ( 1.000000000000000000, 0.000000000000000000, 0.000000000000000000 ) ) ;
#8814 = CARTESIAN_POINT ( 'NONE',  ( 142.6500000000000057, -95.00000000000008527, -186.2999999999999829 ) ) ;
#8815 = DIRECTION ( 'NONE',  ( -1.000000000000000000, 0.000000000000000000, 0.000000000000000000 ) ) ;
#8816 = CIRCLE ( 'NONE', #3496, 2.649999999999985700 ) ;
#8817 = ORIENTED_EDGE ( 'NONE', *, *, #7382, .F. ) ;
#8818 = EDGE_CURVE ( 'NONE', #4036, #5289, #10715, .T. ) ;
#8819 = EDGE_CURVE ( 'NONE', #1387, #11692, #4787, .T. ) ;
#8820 = DIRECTION ( 'NONE',  ( -1.000000000000000000, 0.000000000000000000, 0.000000000000000000 ) ) ;
#8821 = AXIS2_PLACEMENT_3D ( 'NONE', #4570, #3617, #8989 ) ;
#8822 = DIRECTION ( 'NONE',  ( -0.000000000000000000, -0.000000000000000000, -1.000000000000000000 ) ) ;
#8823 = FACE_OUTER_BOUND ( 'NONE', #9939, .T. ) ;
#8824 = DIRECTION ( 'NONE',  ( 0.000000000000000000, 0.000000000000000000, 1.000000000000000000 ) ) ;
#8825 = EDGE_CURVE ( 'NONE', #4156, #14268, #4340, .T. ) ;
#8826 = ORIENTED_EDGE ( 'NONE', *, *, #13208, .T. ) ;
#8827 = CIRCLE ( 'NONE', #4666, 2.649999999999985700 ) ;
#8828 = CARTESIAN_POINT ( 'NONE',  ( 305.0000000000000000, -56.99999999999997158, -169.9999999999999716 ) ) ;
#8829 = COLOUR_RGB ( '',0.8941176470588234615, 0.8941176470588234615, 0.8941176470588234615 ) ;
#8830 = CARTESIAN_POINT ( 'NONE',  ( 219.9999999999999147, -85.00000000000009948, 0.000000000000000000 ) ) ;
#8831 = ORIENTED_EDGE ( 'NONE', *, *, #11365, .T. ) ;
#8832 = CARTESIAN_POINT ( 'NONE',  ( 1.828356344711641102, 3.563200125723180900, -5.433716356636336675E-16 ) ) ;
#8833 = AXIS2_PLACEMENT_3D ( 'NONE', #221, #4683, #4754 ) ;
#8834 = CARTESIAN_POINT ( 'NONE',  ( 228.6602540378443393, -90.00000000000007105, 55.00000000000002132 ) ) ;
#8835 = FACE_OUTER_BOUND ( 'NONE', #5597, .T. ) ;
#8836 = DIRECTION ( 'NONE',  ( 0.000000000000000000, 0.000000000000000000, 1.000000000000000000 ) ) ;
#8837 = ITEM_DEFINED_TRANSFORMATION ( 'NONE', 'NONE', #13465,  #14039 ) ;
#8838 = ORIENTED_EDGE ( 'NONE', *, *, #2375, .T. ) ;
#8839 = DIRECTION ( 'NONE',  ( 0.000000000000000000, 1.224646799147361589E-16, 1.000000000000000000 ) ) ;
#8840 = AXIS2_PLACEMENT_3D ( 'NONE', #5137, #4037, #7365 ) ;
#8841 = VERTEX_POINT ( 'NONE', #3190 ) ;
#8842 = EDGE_CURVE ( 'NONE', #4959, #7600, #11891, .T. ) ;
#8843 = CARTESIAN_POINT ( 'NONE',  ( 236.4999999999999432, -85.00000000000007105, 190.0000000000000000 ) ) ;
#8844 = MECHANICAL_DESIGN_GEOMETRIC_PRESENTATION_REPRESENTATION (  '', ( #6988 ), #5831 ) ;
#8845 = VERTEX_POINT ( 'NONE', #3119 ) ;
#8846 = EDGE_LOOP ( 'NONE', ( #11395, #2137, #10028, #7460 ) ) ;
#8847 = LINE ( 'NONE', #8775, #9644 ) ;
#8848 = UNCERTAINTY_MEASURE_WITH_UNIT (LENGTH_MEASURE( 1.000000000000000082E-05 ), #3641, 'distance_accuracy_value', 'NONE');
#8849 = DIRECTION ( 'NONE',  ( 0.000000000000000000, 0.8660254037844380415, -0.5000000000000011102 ) ) ;
#8850 = CARTESIAN_POINT ( 'NONE',  ( 2.500000000000000000, 2.357898499370433054, -1.951563910473907981E-15 ) ) ;
#8851 = PLANE ( 'NONE',  #13542 ) ;
#8852 = DIRECTION ( 'NONE',  ( -0.000000000000000000, -0.000000000000000000, 1.000000000000000000 ) ) ;
#8853 = FACE_OUTER_BOUND ( 'NONE', #5986, .T. ) ;
#8854 = VECTOR ( 'NONE', #5758, 1000.000000000000000 ) ;
#8855 = DIRECTION ( 'NONE',  ( -1.000000000000000000, -0.000000000000000000, -0.000000000000000000 ) ) ;
#8856 = CONTEXT_DEPENDENT_SHAPE_REPRESENTATION ( #12242, #8681 ) ;
#8857 = DIRECTION ( 'NONE',  ( 0.000000000000000000, 0.000000000000000000, 1.000000000000000000 ) ) ;
#8858 = AXIS2_PLACEMENT_3D ( 'NONE', #12592, #452, #9339 ) ;
#8859 = ORIENTED_EDGE ( 'NONE', *, *, #12694, .F. ) ;
#8860 = STYLED_ITEM ( 'NONE', ( #337 ), #1425 ) ;
#8861 = CIRCLE ( 'NONE', #13256, 2.649999999999985700 ) ;
#8862 = ORIENTED_EDGE ( 'NONE', *, *, #800, .F. ) ;
#8863 = DIRECTION ( 'NONE',  ( 0.000000000000000000, 1.000000000000000000, 0.000000000000000000 ) ) ;
#8864 = ORIENTED_EDGE ( 'NONE', *, *, #13400, .F. ) ;
#8865 = CYLINDRICAL_SURFACE ( 'NONE', #9786, 2.649999999999985700 ) ;
#8866 = VECTOR ( 'NONE', #11221, 1000.000000000000000 ) ;
#8867 = VERTEX_POINT ( 'NONE', #7306 ) ;
#8868 = CARTESIAN_POINT ( 'NONE',  ( 13.50000000000000000, 0.000000000000000000, 186.0000000000000000 ) ) ;
#8869 = ORIENTED_EDGE ( 'NONE', *, *, #8244, .T. ) ;
#8870 = DIRECTION ( 'NONE',  ( -0.000000000000000000, -0.000000000000000000, -1.000000000000000000 ) ) ;
#8871 = FACE_OUTER_BOUND ( 'NONE', #12170, .T. ) ;
#8872 = DIRECTION ( 'NONE',  ( -0.000000000000000000, 1.000000000000000000, 1.224646799147353207E-16 ) ) ;
#8873 = COLOUR_RGB ( '',0.8941176470588234615, 0.8941176470588234615, 0.8941176470588234615 ) ;
#8874 = CARTESIAN_POINT ( 'NONE',  ( 470.0000000000000000, -15.00000000000000000, 240.0000000000000284 ) ) ;
#8875 = EDGE_CURVE ( 'NONE', #1387, #7393, #3443, .T. ) ;
#8876 = DIRECTION ( 'NONE',  ( 1.000000000000000000, 0.000000000000000000, 0.000000000000000000 ) ) ;
#8877 = ADVANCED_FACE ( 'NONE', ( #5361 ), #8463, .F. ) ;
#8878 = LINE ( 'NONE', #3511, #5143 ) ;
#8879 = LINE ( 'NONE', #5331, #844 ) ;
#8880 = CIRCLE ( 'NONE', #13492, 2.500000000000000000 ) ;
#8881 = ORIENTED_EDGE ( 'NONE', *, *, #14078, .T. ) ;
#8882 = VERTEX_POINT ( 'NONE', #6445 ) ;
#8883 = FACE_OUTER_BOUND ( 'NONE', #11268, .T. ) ;
#8884 = EDGE_CURVE ( 'NONE', #8184, #13361, #7095, .T. ) ;
#8885 = DIRECTION ( 'NONE',  ( -0.000000000000000000, -0.000000000000000000, -1.000000000000000000 ) ) ;
#8886 = ORIENTED_EDGE ( 'NONE', *, *, #3049, .F. ) ;
#8887 = DIRECTION ( 'NONE',  ( -0.000000000000000000, 1.000000000000000000, 0.000000000000000000 ) ) ;
#8888 = DIRECTION ( 'NONE',  ( 0.000000000000000000, 1.000000000000000000, 0.000000000000000000 ) ) ;
#8889 = DIRECTION ( 'NONE',  ( 0.000000000000000000, 0.000000000000000000, -1.000000000000000000 ) ) ;
#8890 = ORIENTED_EDGE ( 'NONE', *, *, #1154, .F. ) ;
#8891 = EDGE_CURVE ( 'NONE', #13194, #12598, #11812, .T. ) ;
#8892 = PRODUCT_DEFINITION ( 'UNKNOWN', '', #3322, #13781 ) ;
#8893 = LINE ( 'NONE', #10999, #6280 ) ;
#8894 = LINE ( 'NONE', #13306, #1175 ) ;
#8895 = CARTESIAN_POINT ( 'NONE',  ( -0.2277608394786177770, 1.564486285910743648E-15, -12.77499999999999858 ) ) ;
#8896 = PRODUCT_DEFINITION_SHAPE ( 'NONE', 'NONE',  #5595 ) ;
#8897 = LINE ( 'NONE', #13173, #7165 ) ;
#8898 = ORIENTED_EDGE ( 'NONE', *, *, #6928, .T. ) ;
#8899 = ADVANCED_FACE ( 'NONE', ( #13386 ), #2226, .T. ) ;
#8900 = EDGE_CURVE ( 'NONE', #2542, #2208, #827, .T. ) ;
#8901 = ADVANCED_FACE ( 'NONE', ( #233 ), #1049, .T. ) ;
#8902 = EDGE_CURVE ( 'NONE', #4007, #10967, #3340, .T. ) ;
#8903 = CARTESIAN_POINT ( 'NONE',  ( 303.3333333333333144, -25.00000000000000000, -222.5000000000000853 ) ) ;
#8904 = FACE_BOUND ( 'NONE', #7837, .T. ) ;
#8905 = ORIENTED_EDGE ( 'NONE', *, *, #13377, .F. ) ;
#8906 = CARTESIAN_POINT ( 'NONE',  ( 0.6448876103708359731, 4.246476118072354922, -0.2256878752776725616 ) ) ;
#8907 = ADVANCED_FACE ( 'NONE', ( #12311 ), #11298, .T. ) ;
#8908 = CARTESIAN_POINT ( 'NONE',  ( 0.000000000000000000, 0.000000000000000000, 0.000000000000000000 ) ) ;
#8909 = DIRECTION ( 'NONE',  ( 0.000000000000000000, -0.000000000000000000, 1.000000000000000000 ) ) ;
#8910 = DIRECTION ( 'NONE',  ( 6.123233995736766036E-17, -1.000000000000000000, 0.000000000000000000 ) ) ;
#8911 = ITEM_DEFINED_TRANSFORMATION ( 'NONE', 'NONE', #5397,  #14039 ) ;
#8912 = VERTEX_POINT ( 'NONE', #12162 ) ;
#8913 = CARTESIAN_POINT ( 'NONE',  ( 219.9999999999999716, -20.00000000000000000, 225.1500000000000625 ) ) ;
#8914 = ORIENTED_EDGE ( 'NONE', *, *, #11002, .F. ) ;
#8915 = DIRECTION ( 'NONE',  ( 1.000000000000000000, 0.000000000000000000, 0.000000000000000000 ) ) ;
#8916 = ORIENTED_EDGE ( 'NONE', *, *, #4615, .T. ) ;
#8917 = EDGE_LOOP ( 'NONE', ( #11847, #9782, #13738, #3105 ) ) ;
#8918 = DIRECTION ( 'NONE',  ( 0.000000000000000000, 0.000000000000000000, 1.000000000000000000 ) ) ;
#8919 = DIRECTION ( 'NONE',  ( 0.000000000000000000, 1.000000000000000000, -1.224646799147353207E-16 ) ) ;
#8920 = CONICAL_SURFACE ( 'NONE', #551, 0.8509999999999999787, 0.06981317007976602096 ) ;
#8921 = VECTOR ( 'NONE', #10912, 1000.000000000000000 ) ;
#8922 = DIRECTION ( 'NONE',  ( 0.000000000000000000, -0.000000000000000000, -1.000000000000000000 ) ) ;
#8923 = DIRECTION ( 'NONE',  ( 0.000000000000000000, 0.000000000000000000, -1.000000000000000000 ) ) ;
#8924 = CARTESIAN_POINT ( 'NONE',  ( -31.74999999999995737, 3.061616997868384127E-16, -2.500000000000000888 ) ) ;
#8925 = CARTESIAN_POINT ( 'NONE',  ( 219.9999999999999716, -85.00000000000007105, 64.14213562373096522 ) ) ;
#8926 = EDGE_CURVE ( 'NONE', #3478, #12934, #10130, .T. ) ;
#8927 = CARTESIAN_POINT ( 'NONE',  ( 2.740000000000000213, 0.000000000000000000, 0.000000000000000000 ) ) ;
#8928 = ITEM_DEFINED_TRANSFORMATION ( 'NONE', 'NONE', #13255,  #14039 ) ;
#8929 = CARTESIAN_POINT ( 'NONE',  ( 386.6666666666666288, -20.00000000000000000, -222.5000000000000853 ) ) ;
#8930 = EDGE_LOOP ( 'NONE', ( #5713, #7181 ) ) ;
#8931 = ORIENTED_EDGE ( 'NONE', *, *, #4191, .F. ) ;
#8932 = CARTESIAN_POINT ( 'NONE',  ( 0.9586399445693778443, 0.8293189044373067143, -0.5150000000000000133 ) ) ;
#8933 = VERTEX_POINT ( 'NONE', #5773 ) ;
#8934 = FACE_OUTER_BOUND ( 'NONE', #7281, .T. ) ;
#8935 = ORIENTED_EDGE ( 'NONE', *, *, #11258, .F. ) ;
#8936 = DIRECTION ( 'NONE',  ( -1.000000000000000000, -0.000000000000000000, -0.000000000000000000 ) ) ;
#8937 = ORIENTED_EDGE ( 'NONE', *, *, #13753, .T. ) ;
#8938 = DIRECTION ( 'NONE',  ( 0.000000000000000000, 0.000000000000000000, 1.000000000000000000 ) ) ;
#8939 = CARTESIAN_POINT ( 'NONE',  ( 4.154306624730864428, 2.398490048084778170, -3.721999068284300272 ) ) ;
#8940 = CARTESIAN_POINT ( 'NONE',  ( 8.000000000000000000, -0.5149999999999999023, -1.857513327677604022E-15 ) ) ;
#8941 = DIRECTION ( 'NONE',  ( -0.000000000000000000, -0.000000000000000000, 1.000000000000000000 ) ) ;
#8942 = EDGE_CURVE ( 'NONE', #5507, #2488, #6417, .T. ) ;
#8943 = CARTESIAN_POINT ( 'NONE',  ( 470.0000000000000000, -15.00000000000000000, 205.0000000000000284 ) ) ;
#8944 = CARTESIAN_POINT ( 'NONE',  ( -5.000000000000000888, 8.660254037844390851, 200.0000000000000000 ) ) ;
#8945 = ORIENTED_EDGE ( 'NONE', *, *, #1064, .F. ) ;
#8946 = VERTEX_POINT ( 'NONE', #1119 ) ;
#8947 = EDGE_CURVE ( 'NONE', #7175, #10685, #11504, .T. ) ;
#8948 = DIRECTION ( 'NONE',  ( -0.000000000000000000, 1.000000000000000000, 1.224646799147353207E-16 ) ) ;
#8949 = EDGE_LOOP ( 'NONE', ( #4017, #5217, #14204, #5277 ) ) ;
#8950 = CARTESIAN_POINT ( 'NONE',  ( 470.0000000000000000, -20.00000000000000000, 250.0000000000000000 ) ) ;
#8951 = CARTESIAN_POINT ( 'NONE',  ( -2.000000000000001776, 0.000000000000000000, 0.000000000000000000 ) ) ;
#8952 = CIRCLE ( 'NONE', #3856, 2.649999999999985700 ) ;
#8953 = AXIS2_PLACEMENT_3D ( 'NONE', #8925, #11037, #2250 ) ;
#8954 = FACE_BOUND ( 'NONE', #10210, .T. ) ;
#8955 = FACE_OUTER_BOUND ( 'NONE', #5431, .T. ) ;
#8956 = AXIS2_PLACEMENT_3D ( 'NONE', #11809, #14048, #7378 ) ;
#8957 = LINE ( 'NONE', #6502, #6218 ) ;
#8958 = CARTESIAN_POINT ( 'NONE',  ( 13.50000000000000000, 0.000000000000000000, 186.0000000000000000 ) ) ;
#8959 = AXIS2_PLACEMENT_3D ( 'NONE', #9546, #13962, #810 ) ;
#8960 = VERTEX_POINT ( 'NONE', #6726 ) ;
#8961 = EDGE_CURVE ( 'NONE', #7287, #1982, #1300, .T. ) ;
#8962 = AXIS2_PLACEMENT_3D ( 'NONE', #1182, #8888, #10181 ) ;
#8963 = CARTESIAN_POINT ( 'NONE',  ( 302.5000000000000000, -36.99999999999997868, -180.0000000000000000 ) ) ;
#8964 = DIRECTION ( 'NONE',  ( 1.000000000000000000, -0.000000000000000000, -0.000000000000000000 ) ) ;
#8965 = VECTOR ( 'NONE', #11128, 1000.000000000000000 ) ;
#8966 = DIRECTION ( 'NONE',  ( -0.000000000000000000, -0.000000000000000000, -1.000000000000000000 ) ) ;
#8967 = EDGE_LOOP ( 'NONE', ( #2755, #10976 ) ) ;
#8968 = AXIS2_PLACEMENT_3D ( 'NONE', #481, #8046, #1509 ) ;
#8969 = AXIS2_PLACEMENT_3D ( 'NONE', #13011, #5256, #8361 ) ;
#8970 = DIRECTION ( 'NONE',  ( 0.000000000000000000, 1.000000000000000000, 0.000000000000000000 ) ) ;
#8971 = ADVANCED_FACE ( 'NONE', ( #1265, #5566 ), #1197, .T. ) ;
#8972 = ADVANCED_FACE ( 'NONE', ( #4489 ), #6867, .T. ) ;
#8973 = DIRECTION ( 'NONE',  ( 0.000000000000000000, 1.000000000000000000, 0.000000000000000000 ) ) ;
#8974 = DIRECTION ( 'NONE',  ( 0.000000000000000000, 0.000000000000000000, 1.000000000000000000 ) ) ;
#8975 = AXIS2_PLACEMENT_3D ( 'NONE', #3092, #12007, #2056 ) ;
#8976 = ADVANCED_FACE ( 'NONE', ( #8871 ), #2474, .F. ) ;
#8977 = AXIS2_PLACEMENT_3D ( 'NONE', #6742, #4569, #10219 ) ;
#8978 = ORIENTED_EDGE ( 'NONE', *, *, #6335, .F. ) ;
#8979 = VECTOR ( 'NONE', #11538, 1000.000000000000000 ) ;
#8980 = FACE_OUTER_BOUND ( 'NONE', #13118, .T. ) ;
#8981 = VERTEX_POINT ( 'NONE', #12378 ) ;
#8982 = FACE_OUTER_BOUND ( 'NONE', #10493, .T. ) ;
#8983 = EDGE_LOOP ( 'NONE', ( #3654, #4517, #11850, #12910 ) ) ;
#8984 = ORIENTED_EDGE ( 'NONE', *, *, #13560, .T. ) ;
#8985 = FACE_OUTER_BOUND ( 'NONE', #9346, .T. ) ;
#8986 = CARTESIAN_POINT ( 'NONE',  ( 303.3333333333333144, -20.00000000000000000, 219.8500000000001080 ) ) ;
#8987 = SURFACE_SIDE_STYLE ('',( #9943 ) ) ;
#8988 = VECTOR ( 'NONE', #8446, 1000.000000000000000 ) ;
#8989 = DIRECTION ( 'NONE',  ( -1.000000000000000000, 0.000000000000000000, 0.000000000000000000 ) ) ;
#8990 = CARTESIAN_POINT ( 'NONE',  ( 0.7826237921249277196, 0.000000000000000000, 0.000000000000000000 ) ) ;
#8991 = LINE ( 'NONE', #2106, #13810 ) ;
#8992 = EDGE_CURVE ( 'NONE', #10379, #3993, #3261, .T. ) ;
#8993 = LINE ( 'NONE', #10973, #12711 ) ;
#8994 = CONTEXT_DEPENDENT_SHAPE_REPRESENTATION ( #539, #6695 ) ;
#8995 = ORIENTED_EDGE ( 'NONE', *, *, #12648, .T. ) ;
#8996 = EDGE_LOOP ( 'NONE', ( #3123, #2779, #3040, #5534 ) ) ;
#8997 = CARTESIAN_POINT ( 'NONE',  ( 305.0000000000000000, -56.99999999999997158, -169.9999999999999716 ) ) ;
#8998 =( REPRESENTATION_RELATIONSHIP ('NONE','NONE', #11251, #208 ) REPRESENTATION_RELATIONSHIP_WITH_TRANSFORMATION ( #4507 )SHAPE_REPRESENTATION_RELATIONSHIP( ) );
#8999 = ORIENTED_EDGE ( 'NONE', *, *, #7206, .F. ) ;
#9000 = DIRECTION ( 'NONE',  ( -0.000000000000000000, -0.000000000000000000, 1.000000000000000000 ) ) ;
#9001 = ADVANCED_FACE ( 'NONE', ( #6585 ), #11012, .F. ) ;
#9002 = VERTEX_POINT ( 'NONE', #8834 ) ;
#9003 = DIRECTION ( 'NONE',  ( -1.000000000000000000, -0.000000000000000000, -0.000000000000000000 ) ) ;
#9004 = VERTEX_POINT ( 'NONE', #2518 ) ;
#9005 = AXIS2_PLACEMENT_3D ( 'NONE', #11244, #1284, #10153 ) ;
#9006 = FACE_BOUND ( 'NONE', #553, .T. ) ;
#9007 = B_SPLINE_CURVE_WITH_KNOTS ( 'NONE', 3,
 ( #2031, #2104, #7610, #3212 ),
 .UNSPECIFIED., .F., .F.,
 ( 4, 4 ),
 ( 0.004656695506220393486, 0.007337072593346777132 ),
 .UNSPECIFIED. ) ;
#9008 = DIRECTION ( 'NONE',  ( -0.000000000000000000, -0.000000000000000000, -1.000000000000000000 ) ) ;
#9009 = CARTESIAN_POINT ( 'NONE',  ( 17.00000000000000000, 0.000000000000000000, 0.000000000000000000 ) ) ;
#9010 = LINE ( 'NONE', #2343, #8921 ) ;
#9011 = DIRECTION ( 'NONE',  ( 0.000000000000000000, 1.000000000000000000, -1.287488025362403787E-15 ) ) ;
#9012 = DIRECTION ( 'NONE',  ( 1.000000000000000000, 0.000000000000000000, 0.000000000000000000 ) ) ;
#9013 = ORIENTED_EDGE ( 'NONE', *, *, #3644, .T. ) ;
#9014 = AXIS2_PLACEMENT_3D ( 'NONE', #5994, #10420, #7012 ) ;
#9015 = VERTEX_POINT ( 'NONE', #12522 ) ;
#9016 = ORIENTED_EDGE ( 'NONE', *, *, #11656, .T. ) ;
#9017 = CARTESIAN_POINT ( 'NONE',  ( 4.154306624730763176, -2.398490048084970461, -3.721999068284303824 ) ) ;
#9018 = EDGE_CURVE ( 'NONE', #12143, #1416, #595, .T. ) ;
#9019 = ORIENTED_EDGE ( 'NONE', *, *, #7283, .F. ) ;
#9020 = DIRECTION ( 'NONE',  ( 0.000000000000000000, -1.000000000000000000, 1.287488025362403787E-15 ) ) ;
#9021 = DIRECTION ( 'NONE',  ( -0.000000000000000000, -0.000000000000000000, 1.000000000000000000 ) ) ;
#9022 = CARTESIAN_POINT ( 'NONE',  ( 8.000000000000000000, -0.5149999999999999023, -1.857513327677604022E-15 ) ) ;
#9023 = CIRCLE ( 'NONE', #5108, 2.649999999999985700 ) ;
#9024 = DIRECTION ( 'NONE',  ( -0.000000000000000000, -0.000000000000000000, -1.000000000000000000 ) ) ;
#9025 = DIRECTION ( 'NONE',  ( -0.000000000000000000, -0.000000000000000000, -1.000000000000000000 ) ) ;
#9026 = EDGE_CURVE ( 'NONE', #11223, #12345, #9898, .T. ) ;
#9027 = LINE ( 'NONE', #7065, #2544 ) ;
#9028 = DIRECTION ( 'NONE',  ( 0.000000000000000000, 0.000000000000000000, -1.000000000000000000 ) ) ;
#9029 = ORIENTED_EDGE ( 'NONE', *, *, #10040, .T. ) ;
#9030 = CIRCLE ( 'NONE', #5560, 4.000000000000000000 ) ;
#9031 = LINE ( 'NONE', #3531, #6049 ) ;
#9032 = AXIS2_PLACEMENT_3D ( 'NONE', #10958, #14203, #8629 ) ;
#9033 = CARTESIAN_POINT ( 'NONE',  ( 4.999999999999993783, 8.660254037844390851, -200.0000000000000000 ) ) ;
#9034 = CARTESIAN_POINT ( 'NONE',  ( 1.799999999999996048, 1.249139735130300365E-15, 10.20000000000000107 ) ) ;
#9035 = ORIENTED_EDGE ( 'NONE', *, *, #3309, .T. ) ;
#9036 = CARTESIAN_POINT ( 'NONE',  ( 305.0000000000000000, -56.99999999999997158, -180.0000000000000000 ) ) ;
#9037 = EDGE_CURVE ( 'NONE', #663, #8115, #3864, .T. ) ;
#9038 = CARTESIAN_POINT ( 'NONE',  ( 82.99999999999998579, 8.660254037844390851, 200.0000000000000000 ) ) ;
#9039 = DIRECTION ( 'NONE',  ( -1.000000000000000000, -6.123233995736766036E-17, -6.123233995736764803E-17 ) ) ;
#9040 = ADVANCED_FACE ( 'NONE', ( #4844 ), #6932, .F. ) ;
#9041 = AXIS2_PLACEMENT_3D ( 'NONE', #1637, #4853, #13684 ) ;
#9042 = CIRCLE ( 'NONE', #2087, 2.500000000000002220 ) ;
#9043 = CONTEXT_DEPENDENT_SHAPE_REPRESENTATION ( #73, #10525 ) ;
#9044 = AXIS2_PLACEMENT_3D ( 'NONE', #13537, #106, #12326 ) ;
#9045 = ORIENTED_EDGE ( 'NONE', *, *, #110, .T. ) ;
#9046 = DIRECTION ( 'NONE',  ( 0.000000000000000000, -1.000000000000000000, 0.000000000000000000 ) ) ;
#9047 = ORIENTED_EDGE ( 'NONE', *, *, #3485, .T. ) ;
#9048 = DIRECTION ( 'NONE',  ( -0.000000000000000000, -0.000000000000000000, 1.000000000000000000 ) ) ;
#9049 = ADVANCED_FACE ( 'NONE', ( #2735 ), #3676, .F. ) ;
#9050 = VECTOR ( 'NONE', #897, 1000.000000000000000 ) ;
#9051 = EDGE_LOOP ( 'NONE', ( #4157, #4736, #4415, #8890 ) ) ;
#9052 = ORIENTED_EDGE ( 'NONE', *, *, #1610, .F. ) ;
#9053 = LINE ( 'NONE', #7748, #5022 ) ;
#9054 = DIRECTION ( 'NONE',  ( 0.000000000000000000, -0.8660254037844390407, -0.4999999999999994449 ) ) ;
#9055 = APPLICATION_CONTEXT ( 'automotive_design' ) ;
#9056 = DIRECTION ( 'NONE',  ( 0.000000000000000000, 0.000000000000000000, 1.000000000000000000 ) ) ;
#9057 = AXIS2_PLACEMENT_3D ( 'NONE', #12939, #6347, #9755 ) ;
#9058 = EDGE_CURVE ( 'NONE', #14164, #3772, #2588, .T. ) ;
#9059 = CARTESIAN_POINT ( 'NONE',  ( 347.0000000000000000, 8.660254037844390851, 199.9990000000000236 ) ) ;
#9060 = DIRECTION ( 'NONE',  ( -1.000000000000000000, 0.000000000000000000, 0.000000000000000000 ) ) ;
#9061 = DIRECTION ( 'NONE',  ( 1.000000000000000000, 0.000000000000000000, 0.000000000000000000 ) ) ;
#9062 =( LENGTH_UNIT ( ) NAMED_UNIT ( * ) SI_UNIT ( .MILLI., .METRE. ) );
#9063 = CARTESIAN_POINT ( 'NONE',  ( 3.679171394226031122, 2.494631558665830973, -0.3503314178412474389 ) ) ;
#9064 = TOROIDAL_SURFACE ( 'NONE', #9771, 4.000000000000000000, 0.2500000000000000000 ) ;
#9065 = ORIENTED_EDGE ( 'NONE', *, *, #13449, .T. ) ;
#9066 = ORIENTED_EDGE ( 'NONE', *, *, #3817, .T. ) ;
#9067 = CARTESIAN_POINT ( 'NONE',  ( 2.500000000000000000, 2.357898499370433054, -1.951563910473907981E-15 ) ) ;
#9068 = ORIENTED_EDGE ( 'NONE', *, *, #7615, .F. ) ;
#9069 = FACE_OUTER_BOUND ( 'NONE', #2618, .T. ) ;
#9070 = ADVANCED_FACE ( 'NONE', ( #7010 ), #4914, .F. ) ;
#9071 = VERTEX_POINT ( 'NONE', #10496 ) ;
#9072 = EDGE_CURVE ( 'NONE', #791, #12703, #11279, .T. ) ;
#9073 = DIRECTION ( 'NONE',  ( -1.000000000000000000, -0.000000000000000000, -0.000000000000000000 ) ) ;
#9074 = VERTEX_POINT ( 'NONE', #1626 ) ;
#9075 = CARTESIAN_POINT ( 'NONE',  ( 305.0000000000000000, -56.99999999999997158, -169.9999999999999716 ) ) ;
#9076 = LINE ( 'NONE', #12915, #9903 ) ;
#9077 = AXIS2_PLACEMENT_3D ( 'NONE', #315, #6952, #12470 ) ;
#9078 = FILL_AREA_STYLE ('',( #1376 ) ) ;
#9079 = CIRCLE ( 'NONE', #6729, 13.50000000000000000 ) ;
#9080 = ADVANCED_FACE ( 'NONE', ( #1552 ), #3602, .F. ) ;
#9081 = CARTESIAN_POINT ( 'NONE',  ( 303.3333333333333144, -20.00000000000000000, 222.5000000000000853 ) ) ;
#9082 = AXIS2_PLACEMENT_3D ( 'NONE', #13106, #12032, #7665 ) ;
#9083 = AXIS2_PLACEMENT_3D ( 'NONE', #54, #929, #2858 ) ;
#9084 = PRESENTATION_STYLE_ASSIGNMENT (( #6105 ) ) ;
#9085 =( LENGTH_UNIT ( ) NAMED_UNIT ( * ) SI_UNIT ( .MILLI., .METRE. ) );
#9086 = DIRECTION ( 'NONE',  ( 0.000000000000000000, 0.000000000000000000, -1.000000000000000000 ) ) ;
#9087 = ORIENTED_EDGE ( 'NONE', *, *, #6032, .F. ) ;
#9088 = EDGE_LOOP ( 'NONE', ( #2308, #718, #14020, #12697 ) ) ;
#9089 = AXIS2_PLACEMENT_3D ( 'NONE', #1474, #1405, #11150 ) ;
#9090 = ORIENTED_EDGE ( 'NONE', *, *, #9578, .F. ) ;
#9091 = DIRECTION ( 'NONE',  ( 1.000000000000000000, -0.000000000000000000, 0.000000000000000000 ) ) ;
#9092 = ORIENTED_EDGE ( 'NONE', *, *, #2881, .F. ) ;
#9093 = MECHANICAL_DESIGN_GEOMETRIC_PRESENTATION_REPRESENTATION (  '', ( #10484 ), #12107 ) ;
#9094 = ORIENTED_EDGE ( 'NONE', *, *, #980, .F. ) ;
#9095 = FACE_OUTER_BOUND ( 'NONE', #1484, .T. ) ;
#9096 = CIRCLE ( 'NONE', #10732, 10.72500000000000142 ) ;
#9097 = ORIENTED_EDGE ( 'NONE', *, *, #2035, .F. ) ;
#9098 = PLANE ( 'NONE',  #7794 ) ;
#9099 = DIRECTION ( 'NONE',  ( 0.000000000000000000, 0.000000000000000000, -1.000000000000000000 ) ) ;
#9100 = AXIS2_PLACEMENT_3D ( 'NONE', #13960, #2943, #1763 ) ;
#9101 = CARTESIAN_POINT ( 'NONE',  ( 2.500000000000000000, 0.000000000000000000, 0.000000000000000000 ) ) ;
#9102 = DIRECTION ( 'NONE',  ( -1.000000000000000000, 0.000000000000000000, 0.000000000000000000 ) ) ;
#9103 = CARTESIAN_POINT ( 'NONE',  ( -13.50000000000000000, 0.000000000000000000, -186.0000000000000000 ) ) ;
#9104 = DIRECTION ( 'NONE',  ( -1.000000000000000000, 0.000000000000000000, 0.000000000000000000 ) ) ;
#9105 = DIRECTION ( 'NONE',  ( -1.000000000000000000, 0.000000000000000000, -0.000000000000000000 ) ) ;
#9106 = EDGE_CURVE ( 'NONE', #7861, #13795, #1479, .T. ) ;
#9107 = VERTEX_POINT ( 'NONE', #375 ) ;
#9108 = PRESENTATION_STYLE_ASSIGNMENT (( #3669 ) ) ;
#9109 = CYLINDRICAL_SURFACE ( 'NONE', #2344, 2.649999999999985700 ) ;
#9110 = CARTESIAN_POINT ( 'NONE',  ( 4.999999999999999112, -8.660254037844389075, 210.0000000000000000 ) ) ;
#9111 = CARTESIAN_POINT ( 'NONE',  ( 145.5000000000000284, -95.00000000000008527, -190.0000000000000000 ) ) ;
#9112 = VERTEX_POINT ( 'NONE', #7221 ) ;
#9113 = DIRECTION ( 'NONE',  ( -0.000000000000000000, 0.000000000000000000, -1.000000000000000000 ) ) ;
#9114 = CARTESIAN_POINT ( 'NONE',  ( 2.740000000000000213, 0.000000000000000000, 0.000000000000000000 ) ) ;
#9115 = DIRECTION ( 'NONE',  ( 0.000000000000000000, 0.000000000000000000, 1.000000000000000000 ) ) ;
#9116 = EDGE_CURVE ( 'NONE', #13005, #2622, #6135, .T. ) ;
#9117 = EDGE_LOOP ( 'NONE', ( #3868, #2093, #11676, #2852 ) ) ;
#9118 = DIRECTION ( 'NONE',  ( 0.000000000000000000, -0.000000000000000000, 1.000000000000000000 ) ) ;
#9119 = PRODUCT_DEFINITION_SHAPE ( 'NONE', 'NONE',  #8151 ) ;
#9120 = VERTEX_POINT ( 'NONE', #5064 ) ;
#9121 = CARTESIAN_POINT ( 'NONE',  ( 3.455068668934414777, -2.624017327439094327, -3.316620875263732504 ) ) ;
#9122 = ADVANCED_FACE ( 'NONE', ( #6066 ), #3813, .T. ) ;
#9123 = EDGE_CURVE ( 'NONE', #13461, #12113, #10341, .T. ) ;
#9124 = ORIENTED_EDGE ( 'NONE', *, *, #12783, .F. ) ;
#9125 = EDGE_LOOP ( 'NONE', ( #9094, #9723, #2560, #5246 ) ) ;
#9126 = FACE_BOUND ( 'NONE', #14100, .T. ) ;
#9127 = CARTESIAN_POINT ( 'NONE',  ( -1.390230914382372118, -4.043987460488664532, -3.502507215260523665 ) ) ;
#9128 = CARTESIAN_POINT ( 'NONE',  ( -299.9999999999999432, -75.00000000000008527, 10.00000000000000178 ) ) ;
#9129 = DIRECTION ( 'NONE',  ( -0.000000000000000000, -0.000000000000000000, 1.000000000000000000 ) ) ;
#9130 = CARTESIAN_POINT ( 'NONE',  ( 0.000000000000000000, 0.000000000000000000, -4.974599999999998801 ) ) ;
#9131 = DIRECTION ( 'NONE',  ( -0.000000000000000000, -0.000000000000000000, 1.000000000000000000 ) ) ;
#9132 = CARTESIAN_POINT ( 'NONE',  ( 4.000000000000000000, 2.309401076758515803, -0.4999999999999995559 ) ) ;
#9133 = ORIENTED_EDGE ( 'NONE', *, *, #1948, .F. ) ;
#9134 = ORIENTED_EDGE ( 'NONE', *, *, #8842, .F. ) ;
#9135 = FACE_OUTER_BOUND ( 'NONE', #12146, .T. ) ;
#9136 = VERTEX_POINT ( 'NONE', #4984 ) ;
#9137 = CARTESIAN_POINT ( 'NONE',  ( 119.9999999999999147, -20.00000000000000000, -169.9999999999999716 ) ) ;
#9138 = ADVANCED_FACE ( 'NONE', ( #12591 ), #2654, .F. ) ;
#9139 = EDGE_CURVE ( 'NONE', #4036, #12837, #449, .T. ) ;
#9140 = CLOSED_SHELL ( 'NONE', ( #13154, #11889, #3539, #3357, #1792, #12529, #12429, #4203, #6567, #2217, #9916, #12604 ) ) ;
#9141 = EDGE_LOOP ( 'NONE', ( #10747, #14088 ) ) ;
#9142 = DIRECTION ( 'NONE',  ( 1.000000000000000000, 0.000000000000000000, -0.000000000000000000 ) ) ;
#9143 = ORIENTED_EDGE ( 'NONE', *, *, #4909, .F. ) ;
#9144 = PLANE ( 'NONE',  #8226 ) ;
#9145 = DIRECTION ( 'NONE',  ( -1.000000000000000000, 0.000000000000000000, 0.000000000000000000 ) ) ;
#9146 = ORIENTED_EDGE ( 'NONE', *, *, #13739, .F. ) ;
#9147 = DIRECTION ( 'NONE',  ( 0.000000000000000000, 0.000000000000000000, 1.000000000000000000 ) ) ;
#9148 = FACE_OUTER_BOUND ( 'NONE', #398, .T. ) ;
#9149 = LINE ( 'NONE', #11980, #8577 ) ;
#9150 = APPLICATION_PROTOCOL_DEFINITION ( 'draft international standard', 'automotive_design', 1998, #9538 ) ;
#9151 = ADVANCED_FACE ( 'NONE', ( #8450 ), #887, .F. ) ;
#9152 = EDGE_CURVE ( 'NONE', #9376, #13709, #6277, .T. ) ;
#9153 = DIRECTION ( 'NONE',  ( 0.000000000000000000, 1.000000000000000000, 0.000000000000000000 ) ) ;
#9154 = EDGE_LOOP ( 'NONE', ( #13521, #10632, #11511, #5465 ) ) ;
#9155 = CONICAL_SURFACE ( 'NONE', #9854, 4.000000000000000000, 0.8911886515913786111 ) ;
#9156 = ADVANCED_FACE ( 'NONE', ( #9769 ), #2953, .F. ) ;
#9157 = EDGE_LOOP ( 'NONE', ( #8817, #3473 ) ) ;
#9158 = ORIENTED_EDGE ( 'NONE', *, *, #14294, .F. ) ;
#9159 = CARTESIAN_POINT ( 'NONE',  ( 469.9999999999998863, -225.0000000000000000, 190.0000000000000000 ) ) ;
#9160 = ORIENTED_EDGE ( 'NONE', *, *, #11810, .F. ) ;
#9161 = DIRECTION ( 'NONE',  ( -1.000000000000000000, 0.000000000000000000, 0.000000000000000000 ) ) ;
#9162 = VERTEX_POINT ( 'NONE', #13025 ) ;
#9163 = DIRECTION ( 'NONE',  ( -1.000000000000000000, -0.000000000000000000, -0.000000000000000000 ) ) ;
#9164 = VECTOR ( 'NONE', #8870, 1000.000000000000000 ) ;
#9165 = CARTESIAN_POINT ( 'NONE',  ( 1.734723475976807094E-15, 4.618802153517012954, -0.4999999999999995559 ) ) ;
#9166 = DIRECTION ( 'NONE',  ( 0.000000000000000000, -1.000000000000000000, 0.000000000000000000 ) ) ;
#9167 = SURFACE_STYLE_USAGE ( .BOTH. , #1690 ) ;
#9168 = DIRECTION ( 'NONE',  ( -0.000000000000000000, -0.000000000000000000, -1.000000000000000000 ) ) ;
#9169 = CARTESIAN_POINT ( 'NONE',  ( 2.500000000000000000, 2.357898499370433054, -1.951563910473907981E-15 ) ) ;
#9170 = ORIENTED_EDGE ( 'NONE', *, *, #13243, .F. ) ;
#9171 = AXIS2_PLACEMENT_3D ( 'NONE', #12114, #6671, #1134 ) ;
#9172 = AXIS2_PLACEMENT_3D ( 'NONE', #2315, #8849, #6460 ) ;
#9173 = LINE ( 'NONE', #13021, #1057 ) ;
#9174 = CYLINDRICAL_SURFACE ( 'NONE', #12803, 4.250000000000000000 ) ;
#9175 = CYLINDRICAL_SURFACE ( 'NONE', #5299, 13.50000000000000000 ) ;
#9176 = CIRCLE ( 'NONE', #5705, 5.000000000000004441 ) ;
#9177 = ADVANCED_FACE ( 'NONE', ( #746 ), #9995, .F. ) ;
#9178 = EDGE_LOOP ( 'NONE', ( #1072, #3364, #12555, #3710 ) ) ;
#9179 = AXIS2_PLACEMENT_3D ( 'NONE', #12030, #12969, #4128 ) ;
#9180 = AXIS2_PLACEMENT_3D ( 'NONE', #537, #311, #4778 ) ;
#9181 = DIRECTION ( 'NONE',  ( 0.000000000000000000, -0.000000000000000000, 1.000000000000000000 ) ) ;
#9182 = VECTOR ( 'NONE', #7852, 1000.000000000000000 ) ;
#9183 = DIRECTION ( 'NONE',  ( 0.000000000000000000, -1.224646799147352714E-16, 1.000000000000000000 ) ) ;
#9184 = CARTESIAN_POINT ( 'NONE',  ( 439.9999999999999432, 0.000000000000000000, 0.000000000000000000 ) ) ;
#9185 =( REPRESENTATION_RELATIONSHIP ('NONE','NONE', #11251, #9307 ) REPRESENTATION_RELATIONSHIP_WITH_TRANSFORMATION ( #9283 )SHAPE_REPRESENTATION_RELATIONSHIP( ) );
#9186 = DIRECTION ( 'NONE',  ( -1.000000000000000000, 0.000000000000000000, 0.000000000000000000 ) ) ;
#9187 = CIRCLE ( 'NONE', #4104, 2.500000000000002220 ) ;
#9188 = VERTEX_POINT ( 'NONE', #957 ) ;
#9189 = LINE ( 'NONE', #8314, #3482 ) ;
#9190 = VECTOR ( 'NONE', #9752, 1000.000000000000000 ) ;
#9191 = EDGE_LOOP ( 'NONE', ( #6055, #5115, #7431, #1362 ) ) ;
#9192 = LINE ( 'NONE', #5074, #1393 ) ;
#9193 = AXIS2_PLACEMENT_3D ( 'NONE', #4303, #14299, #2689 ) ;
#9194 = VECTOR ( 'NONE', #4022, 1000.000000000000000 ) ;
#9195 = ORIENTED_EDGE ( 'NONE', *, *, #9345, .T. ) ;
#9196 = VERTEX_POINT ( 'NONE', #8528 ) ;
#9197 = FACE_OUTER_BOUND ( 'NONE', #13378, .T. ) ;
#9198 = CARTESIAN_POINT ( 'NONE',  ( -0.02511973781850462134, 4.877415612947412882, -3.751298745799839462 ) ) ;
#9199 = AXIS2_PLACEMENT_3D ( 'NONE', #1617, #9391, #5199 ) ;
#9200 = FACE_OUTER_BOUND ( 'NONE', #9125, .T. ) ;
#9201 = CARTESIAN_POINT ( 'NONE',  ( 219.9999999999999716, -85.00000000000007105, 169.9999999999999716 ) ) ;
#9202 = VECTOR ( 'NONE', #5792, 1000.000000000000000 ) ;
#9203 = DIRECTION ( 'NONE',  ( -0.000000000000000000, -0.000000000000000000, -1.000000000000000000 ) ) ;
#9204 = CARTESIAN_POINT ( 'NONE',  ( 307.5000000000000000, -56.99999999999997158, -169.9999999999999716 ) ) ;
#9205 = DIRECTION ( 'NONE',  ( -0.000000000000000000, 1.000000000000000000, -0.000000000000000000 ) ) ;
#9206 = EDGE_CURVE ( 'NONE', #898, #8606, #12951, .T. ) ;
#9207 = CONTEXT_DEPENDENT_SHAPE_REPRESENTATION ( #8441, #12724 ) ;
#9208 = AXIS2_PLACEMENT_3D ( 'NONE', #9256, #12812, #2879 ) ;
#9209 = AXIS2_PLACEMENT_3D ( 'NONE', #6600, #11031, #1061 ) ;
#9210 = ORIENTED_EDGE ( 'NONE', *, *, #7793, .T. ) ;
#9211 = VERTEX_POINT ( 'NONE', #12877 ) ;
#9212 = DIRECTION ( 'NONE',  ( -0.5000000000000051070, 0.000000000000000000, 0.8660254037844355990 ) ) ;
#9213 = EDGE_LOOP ( 'NONE', ( #460, #9857, #7734, #5244 ) ) ;
#9214 = CARTESIAN_POINT ( 'NONE',  ( 219.9999999999999716, -25.00000000000000000, 222.5000000000000853 ) ) ;
#9215 = MECHANICAL_DESIGN_GEOMETRIC_PRESENTATION_REPRESENTATION (  '', ( #2232 ), #9697 ) ;
#9216 = EDGE_LOOP ( 'NONE', ( #13646, #11603, #12314, #5010 ) ) ;
#9217 = DIRECTION ( 'NONE',  ( 0.000000000000000000, 0.000000000000000000, 1.000000000000000000 ) ) ;
#9218 = ORIENTED_EDGE ( 'NONE', *, *, #5882, .F. ) ;
#9219 = CARTESIAN_POINT ( 'NONE',  ( 219.9999999999999716, -85.00000000000007105, -250.0009999999999764 ) ) ;
#9220 = VECTOR ( 'NONE', #11635, 1000.000000000000114 ) ;
#9221 = FACE_OUTER_BOUND ( 'NONE', #5822, .T. ) ;
#9222 = VERTEX_POINT ( 'NONE', #6500 ) ;
#9223 = DIRECTION ( 'NONE',  ( 0.000000000000000000, 1.000000000000000000, 0.000000000000000000 ) ) ;
#9224 = CARTESIAN_POINT ( 'NONE',  ( -6.259644161404860030E-16, -4.618802153517027165, -3.433295621305388234 ) ) ;
#9225 =( LENGTH_UNIT ( ) NAMED_UNIT ( * ) SI_UNIT ( .MILLI., .METRE. ) );
#9226 = DIRECTION ( 'NONE',  ( 1.000000000000000000, 0.000000000000000000, 0.000000000000000000 ) ) ;
#9227 = EDGE_CURVE ( 'NONE', #14079, #4256, #2125, .T. ) ;
#9228 = CONTEXT_DEPENDENT_SHAPE_REPRESENTATION ( #400, #5536 ) ;
#9229 = CARTESIAN_POINT ( 'NONE',  ( 297.3499999999999659, -75.00000000000008527, -186.2999999999999829 ) ) ;
#9230 = EDGE_LOOP ( 'NONE', ( #13505, #8318, #2880, #5182, #2856, #6853 ) ) ;
#9231 = ORIENTED_EDGE ( 'NONE', *, *, #14027, .T. ) ;
#9232 = EDGE_LOOP ( 'NONE', ( #11843, #13985 ) ) ;
#9233 = VECTOR ( 'NONE', #7352, 1000.000000000000000 ) ;
#9234 = ADVANCED_FACE ( 'NONE', ( #3106, #3963, #4257, #1773, #9476, #1993, #3028, #14033 ), #8672, .F. ) ;
#9235 = FACE_BOUND ( 'NONE', #12023, .T. ) ;
#9236 = ORIENTED_EDGE ( 'NONE', *, *, #12004, .F. ) ;
#9237 = CARTESIAN_POINT ( 'NONE',  ( 2.500000000000000444, 0.000000000000000000, -25.03750572909317285 ) ) ;
#9238 = ORIENTED_EDGE ( 'NONE', *, *, #765, .T. ) ;
#9239 = DIRECTION ( 'NONE',  ( 0.000000000000000000, -0.000000000000000000, 1.000000000000000000 ) ) ;
#9240 = ADVANCED_FACE ( 'NONE', ( #11872 ), #13090, .F. ) ;
#9241 = EDGE_CURVE ( 'NONE', #2854, #1558, #6356, .T. ) ;
#9242 =( LENGTH_UNIT ( ) NAMED_UNIT ( * ) SI_UNIT ( .MILLI., .METRE. ) );
#9243 = DIRECTION ( 'NONE',  ( -1.000000000000000000, 0.000000000000000000, 0.000000000000000000 ) ) ;
#9244 = CARTESIAN_POINT ( 'NONE',  ( 0.000000000000000000, 0.000000000000000000, 0.000000000000000000 ) ) ;
#9245 = FILL_AREA_STYLE ('',( #1396 ) ) ;
#9246 = VECTOR ( 'NONE', #7889, 1000.000000000000000 ) ;
#9247 = ADVANCED_FACE ( 'NONE', ( #13968 ), #2882, .F. ) ;
#9248 = DIRECTION ( 'NONE',  ( -0.5000000000000016653, 0.8660254037844378194, 0.000000000000000000 ) ) ;
#9249 = PRODUCT_DEFINITION_SHAPE ( 'NONE', 'NONE',  #14309 ) ;
#9250 = CARTESIAN_POINT ( 'NONE',  ( 2.500000000000000000, 0.000000000000000000, 0.000000000000000000 ) ) ;
#9251 = ORIENTED_EDGE ( 'NONE', *, *, #5510, .F. ) ;
#9252 = DIRECTION ( 'NONE',  ( 0.000000000000000000, 0.000000000000000000, 1.000000000000000000 ) ) ;
#9253 = AXIS2_PLACEMENT_3D ( 'NONE', #1044, #8973, #8909 ) ;
#9254 = FACE_OUTER_BOUND ( 'NONE', #2158, .T. ) ;
#9255 = ADVANCED_FACE ( 'NONE', ( #4183 ), #8600, .F. ) ;
#9256 = CARTESIAN_POINT ( 'NONE',  ( 0.000000000000000000, 0.000000000000000000, 0.000000000000000000 ) ) ;
#9257 = ORIENTED_EDGE ( 'NONE', *, *, #9935, .F. ) ;
#9258 = ADVANCED_FACE ( 'NONE', ( #10863 ), #673, .T. ) ;
#9259 = DIRECTION ( 'NONE',  ( 1.000000000000000000, 0.000000000000000000, 0.000000000000000000 ) ) ;
#9260 = ADVANCED_FACE ( 'NONE', ( #12222, #8954, #4475, #12296 ), #13372, .T. ) ;
#9261 = DIRECTION ( 'NONE',  ( 0.000000000000000000, -1.000000000000000000, 0.000000000000000000 ) ) ;
#9262 = CARTESIAN_POINT ( 'NONE',  ( 88.00000000000000000, 0.000000000000000000, 188.0000000000000000 ) ) ;
#9263 = AXIS2_PLACEMENT_3D ( 'NONE', #5347, #5416, #13170 ) ;
#9264 = DIRECTION ( 'NONE',  ( 0.000000000000000000, -1.000000000000000000, -3.491481338843133355E-15 ) ) ;
#9265 = ADVANCED_FACE ( 'NONE', ( #7856 ), #5552, .T. ) ;
#9266 = AXIS2_PLACEMENT_3D ( 'NONE', #7529, #4352, #11967 ) ;
#9267 = ORIENTED_EDGE ( 'NONE', *, *, #5510, .T. ) ;
#9268 = DIRECTION ( 'NONE',  ( -0.000000000000000000, -0.000000000000000000, 1.000000000000000000 ) ) ;
#9269 = PRESENTATION_LAYER_ASSIGNMENT (  '', '', ( #12541 ) ) ;
#9270 = FACE_OUTER_BOUND ( 'NONE', #1788, .T. ) ;
#9271 = ORIENTED_EDGE ( 'NONE', *, *, #13042, .F. ) ;
#9272 = DIRECTION ( 'NONE',  ( -0.000000000000000000, -0.000000000000000000, -1.000000000000000000 ) ) ;
#9273 = LINE ( 'NONE', #8172, #7318 ) ;
#9274 =( REPRESENTATION_RELATIONSHIP ('NONE','NONE', #11251, #13104 ) REPRESENTATION_RELATIONSHIP_WITH_TRANSFORMATION ( #8110 )SHAPE_REPRESENTATION_RELATIONSHIP( ) );
#9275 = VECTOR ( 'NONE', #5486, 1000.000000000000000 ) ;
#9276 = DIRECTION ( 'NONE',  ( 0.000000000000000000, 0.000000000000000000, 1.000000000000000000 ) ) ;
#9277 = DIRECTION ( 'NONE',  ( 1.007709689656716938E-16, 1.153406566473941260E-16, -1.000000000000000000 ) ) ;
#9278 = FACE_OUTER_BOUND ( 'NONE', #4300, .T. ) ;
#9279 = DIRECTION ( 'NONE',  ( 0.000000000000000000, 1.000000000000000000, 0.000000000000000000 ) ) ;
#9280 = PRESENTATION_STYLE_ASSIGNMENT (( #8106 ) ) ;
#9281 = AXIS2_PLACEMENT_3D ( 'NONE', #13405, #314, #8029 ) ;
#9282 = FACE_OUTER_BOUND ( 'NONE', #1487, .T. ) ;
#9283 = ITEM_DEFINED_TRANSFORMATION ( 'NONE', 'NONE', #1908,  #14039 ) ;
#9284 = EDGE_LOOP ( 'NONE', ( #12632, #11576 ) ) ;
#9285 = EDGE_CURVE ( 'NONE', #1872, #13005, #2146, .T. ) ;
#9286 = EDGE_LOOP ( 'NONE', ( #984, #12419, #7807, #13217 ) ) ;
#9287 = DIRECTION ( 'NONE',  ( -1.000000000000000000, -0.000000000000000000, -0.000000000000000000 ) ) ;
#9288 = VECTOR ( 'NONE', #3184, 1000.000000000000000 ) ;
#9289 = ORIENTED_EDGE ( 'NONE', *, *, #2595, .T. ) ;
#9290 = DIRECTION ( 'NONE',  ( -0.000000000000000000, 0.000000000000000000, 1.000000000000000000 ) ) ;
#9291 = DIRECTION ( 'NONE',  ( 0.000000000000000000, -0.5000000000000009992, -0.8660254037844380415 ) ) ;
#9292 = ORIENTED_EDGE ( 'NONE', *, *, #2246, .T. ) ;
#9293 = LINE ( 'NONE', #12620, #10840 ) ;
#9294 = VERTEX_POINT ( 'NONE', #5686 ) ;
#9295 = CIRCLE ( 'NONE', #10928, 4.000000000000000000 ) ;
#9296 = CARTESIAN_POINT ( 'NONE',  ( 0.000000000000000000, 0.000000000000000000, 0.000000000000000000 ) ) ;
#9297 = DIRECTION ( 'NONE',  ( -1.000000000000000000, -0.000000000000000000, -0.000000000000000000 ) ) ;
#9298 = ORIENTED_EDGE ( 'NONE', *, *, #2537, .F. ) ;
#9299 = DIRECTION ( 'NONE',  ( -1.000000000000000000, 0.000000000000000000, 0.000000000000000000 ) ) ;
#9300 = LINE ( 'NONE', #274, #168 ) ;
#9301 = AXIS2_PLACEMENT_3D ( 'NONE', #14106, #7441, #13890 ) ;
#9302 = FILL_AREA_STYLE ('',( #2484 ) ) ;
#9303 = APPLICATION_PROTOCOL_DEFINITION ( 'draft international standard', 'automotive_design', 1998, #10547 ) ;
#9304 = CARTESIAN_POINT ( 'NONE',  ( 140.0000000000000000, -95.00000000000008527, 190.0000000000000000 ) ) ;
#9305 = ORIENTED_EDGE ( 'NONE', *, *, #6064, .F. ) ;
#9306 = FACE_BOUND ( 'NONE', #2473, .T. ) ;
#9307 = SHAPE_REPRESENTATION ( 'hex flange nut gradea_iso_ISO - 4161 - M5 - N', ( #14039 ), #1206 ) ;
#9308 = ORIENTED_EDGE ( 'NONE', *, *, #14016, .F. ) ;
#9309 = DIRECTION ( 'NONE',  ( 0.000000000000000000, 0.000000000000000000, 1.000000000000000000 ) ) ;
#9310 = TOROIDAL_SURFACE ( 'NONE', #12788, 4.300000000000001599, 0.4499999999999985678 ) ;
#9311 = VERTEX_POINT ( 'NONE', #9983 ) ;
#9312 = CARTESIAN_POINT ( 'NONE',  ( 2.500000000000000000, 1.768423874527822459, -1.021000000000002794 ) ) ;
#9313 = ORIENTED_EDGE ( 'NONE', *, *, #12397, .F. ) ;
#9314 = EDGE_CURVE ( 'NONE', #1382, #4602, #3454, .T. ) ;
#9315 = CARTESIAN_POINT ( 'NONE',  ( -124.9999999999999432, -105.0000000000000853, 40.00000000000000000 ) ) ;
#9316 = ADVANCED_FACE ( 'NONE', ( #7785 ), #13443, .F. ) ;
#9317 = SURFACE_SIDE_STYLE ('',( #13731 ) ) ;
#9318 = CARTESIAN_POINT ( 'NONE',  ( 206.1500000000000057, -85.00000000000007105, 55.00000000000001421 ) ) ;
#9319 = DIRECTION ( 'NONE',  ( -1.000000000000000000, -0.000000000000000000, -0.000000000000000000 ) ) ;
#9320 = CARTESIAN_POINT ( 'NONE',  ( -12.00000000000000000, 0.000000000000000000, 186.0000000000000000 ) ) ;
#9321 = DIRECTION ( 'NONE',  ( -0.8660254037844377084, -0.5000000000000015543, 0.000000000000000000 ) ) ;
#9322 = VECTOR ( 'NONE', #13907, 999.9999999999998863 ) ;
#9323 = ORIENTED_EDGE ( 'NONE', *, *, #13310, .T. ) ;
#9324 = ORIENTED_EDGE ( 'NONE', *, *, #2196, .T. ) ;
#9325 = AXIS2_PLACEMENT_3D ( 'NONE', #10721, #6070, #13029 ) ;
#9326 = VECTOR ( 'NONE', #8792, 1000.000000000000000 ) ;
#9327 =( NAMED_UNIT ( * ) SI_UNIT ( $, .STERADIAN. ) SOLID_ANGLE_UNIT ( ) );
#9328 = ORIENTED_EDGE ( 'NONE', *, *, #7382, .T. ) ;
#9329 = DIRECTION ( 'NONE',  ( -1.000000000000000000, -0.000000000000000000, -0.000000000000000000 ) ) ;
#9330 = EDGE_CURVE ( 'NONE', #1971, #11973, #8893, .T. ) ;
#9331 = CARTESIAN_POINT ( 'NONE',  ( 0.2500000000000002220, 0.000000000000000000, 4.000000000000000000 ) ) ;
#9332 = EDGE_CURVE ( 'NONE', #1098, #8981, #10227, .T. ) ;
#9333 = CONICAL_SURFACE ( 'NONE', #3093, 2.041999999999999815, 1.047197551196591858 ) ;
#9334 = DIRECTION ( 'NONE',  ( 0.000000000000000000, 0.000000000000000000, -1.000000000000000000 ) ) ;
#9335 = ORIENTED_EDGE ( 'NONE', *, *, #8258, .F. ) ;
#9336 = CYLINDRICAL_SURFACE ( 'NONE', #13669, 2.500000000000002220 ) ;
#9337 = CARTESIAN_POINT ( 'NONE',  ( 303.3333333333333144, -20.00000000000000000, 222.5000000000000853 ) ) ;
#9338 = CARTESIAN_POINT ( 'NONE',  ( 347.0000000000000000, -8.660254037844389075, 205.0000000000000284 ) ) ;
#9339 = DIRECTION ( 'NONE',  ( 0.000000000000000000, 0.000000000000000000, -1.000000000000000000 ) ) ;
#9340 = DIRECTION ( 'NONE',  ( 0.000000000000000000, -1.000000000000000000, 0.000000000000000000 ) ) ;
#9341 = EDGE_CURVE ( 'NONE', #3667, #1850, #150, .T. ) ;
#9342 = ADVANCED_FACE ( 'NONE', ( #6849 ), #10969, .F. ) ;
#9343 = AXIS2_PLACEMENT_3D ( 'NONE', #6525, #8771, #7528 ) ;
#9344 = EDGE_CURVE ( 'NONE', #10304, #1708, #459, .T. ) ;
#9345 = EDGE_CURVE ( 'NONE', #7698, #10393, #6711, .T. ) ;
#9346 = EDGE_LOOP ( 'NONE', ( #4226, #13342, #96, #736 ) ) ;
#9347 = CARTESIAN_POINT ( 'NONE',  ( 140.0000000000000000, -75.00000000000008527, 190.0000000000000000 ) ) ;
#9348 = DIRECTION ( 'NONE',  ( 1.000000000000000000, 0.000000000000000000, 0.000000000000000000 ) ) ;
#9349 = EDGE_CURVE ( 'NONE', #8755, #4266, #2580, .T. ) ;
#9350 = ORIENTED_EDGE ( 'NONE', *, *, #4096, .T. ) ;
#9351 = DIRECTION ( 'NONE',  ( 0.000000000000000000, 0.000000000000000000, -1.000000000000000000 ) ) ;
#9352 = CARTESIAN_POINT ( 'NONE',  ( -0.5636800770129166693, -4.293361309317430319, -3.531542292955206275 ) ) ;
#9353 = LINE ( 'NONE', #3906, #5980 ) ;
#9354 = DIRECTION ( 'NONE',  ( -0.000000000000000000, 1.000000000000000000, -0.000000000000000000 ) ) ;
#9355 = CARTESIAN_POINT ( 'NONE',  ( -4.000000000000000000, -2.309401076758512694, -5.000000000000000000 ) ) ;
#9356 = DIRECTION ( 'NONE',  ( -1.000000000000000000, 0.000000000000000000, 0.000000000000000000 ) ) ;
#9357 = CARTESIAN_POINT ( 'NONE',  ( 53.33333333333330017, -15.00000000000000000, 222.5000000000000853 ) ) ;
#9358 = ITEM_DEFINED_TRANSFORMATION ( 'NONE', 'NONE', #6777,  #14039 ) ;
#9359 = ORIENTED_EDGE ( 'NONE', *, *, #6857, .F. ) ;
#9360 = DIRECTION ( 'NONE',  ( 0.000000000000000000, 0.000000000000000000, 1.000000000000000000 ) ) ;
#9361 = ORIENTED_EDGE ( 'NONE', *, *, #2960, .T. ) ;
#9362 = FACE_OUTER_BOUND ( 'NONE', #1383, .T. ) ;
#9363 = DIRECTION ( 'NONE',  ( 1.000000000000000000, 0.000000000000000000, 0.000000000000000000 ) ) ;
#9364 = ORIENTED_EDGE ( 'NONE', *, *, #8416, .F. ) ;
#9365 = CARTESIAN_POINT ( 'NONE',  ( -1.747541505913277282, 3.837784562140256650, -3.503702292528906526 ) ) ;
#9366 = ORIENTED_EDGE ( 'NONE', *, *, #8367, .F. ) ;
#9367 = DIRECTION ( 'NONE',  ( 1.000000000000000000, 0.000000000000000000, -0.000000000000000000 ) ) ;
#9368 = LINE ( 'NONE', #12696, #5053 ) ;
#9369 = EDGE_LOOP ( 'NONE', ( #98, #1572, #12209, #1932 ) ) ;
#9370 = EDGE_CURVE ( 'NONE', #12188, #5384, #13244, .T. ) ;
#9371 = CARTESIAN_POINT ( 'NONE',  ( 386.6666666666666288, -15.00000000000000000, 222.5000000000000853 ) ) ;
#9372 =( NAMED_UNIT ( * ) SI_UNIT ( $, .STERADIAN. ) SOLID_ANGLE_UNIT ( ) );
#9373 = DIRECTION ( 'NONE',  ( 0.000000000000000000, 0.000000000000000000, 1.000000000000000000 ) ) ;
#9374 = APPLICATION_PROTOCOL_DEFINITION ( 'draft international standard', 'automotive_design', 1998, #6096 ) ;
#9375 = LINE ( 'NONE', #12628, #5045 ) ;
#9376 = VERTEX_POINT ( 'NONE', #7652 ) ;
#9377 = CARTESIAN_POINT ( 'NONE',  ( -30.00000000000002842, -20.00000000000000000, 240.0000000000000284 ) ) ;
#9378 = VECTOR ( 'NONE', #12126, 1000.000000000000000 ) ;
#9379 = ORIENTED_EDGE ( 'NONE', *, *, #1342, .T. ) ;
#9380 = DIRECTION ( 'NONE',  ( -1.000000000000000000, 0.000000000000000000, -0.000000000000000000 ) ) ;
#9381 = ORIENTED_EDGE ( 'NONE', *, *, #9969, .F. ) ;
#9382 = CARTESIAN_POINT ( 'NONE',  ( 145.5000000000000284, -95.00000000000008527, 190.0000000000000000 ) ) ;
#9383 = VERTEX_POINT ( 'NONE', #12086 ) ;
#9384 = DIRECTION ( 'NONE',  ( -0.000000000000000000, -0.000000000000000000, 1.000000000000000000 ) ) ;
#9385 = CARTESIAN_POINT ( 'NONE',  ( -5.000000000000000888, 8.660254037844390851, 205.0000000000000284 ) ) ;
#9386 = CARTESIAN_POINT ( 'NONE',  ( -219.9999999999999147, -85.00000000000009948, 30.00000000000000000 ) ) ;
#9387 = AXIS2_PLACEMENT_3D ( 'NONE', #8997, #3493, #7896 ) ;
#9388 = CYLINDRICAL_SURFACE ( 'NONE', #5837, 2.500000000000002220 ) ;
#9389 = AXIS2_PLACEMENT_3D ( 'NONE', #10988, #11057, #13292 ) ;
#9390 = CARTESIAN_POINT ( 'NONE',  ( 299.9999999999999432, -95.00000000000008527, -190.0000000000000000 ) ) ;
#9391 = DIRECTION ( 'NONE',  ( -1.000000000000000000, -0.000000000000000000, -0.000000000000000000 ) ) ;
#9392 = ORIENTED_EDGE ( 'NONE', *, *, #5573, .F. ) ;
#9393 = EDGE_CURVE ( 'NONE', #6403, #10296, #1638, .T. ) ;
#9394 = ORIENTED_EDGE ( 'NONE', *, *, #1129, .F. ) ;
#9395 =( LENGTH_UNIT ( ) NAMED_UNIT ( * ) SI_UNIT ( .MILLI., .METRE. ) );
#9396 = ORIENTED_EDGE ( 'NONE', *, *, #12971, .F. ) ;
#9397 = CARTESIAN_POINT ( 'NONE',  ( -2.000000000000001776, 0.000000000000000000, 0.000000000000000000 ) ) ;
#9398 = FACE_OUTER_BOUND ( 'NONE', #10957, .T. ) ;
#9399 =( NAMED_UNIT ( * ) PLANE_ANGLE_UNIT ( ) SI_UNIT ( $, .RADIAN. ) );
#9400 = EDGE_LOOP ( 'NONE', ( #2964, #3396 ) ) ;
#9401 = DIRECTION ( 'NONE',  ( -0.000000000000000000, -0.000000000000000000, -1.000000000000000000 ) ) ;
#9402 = AXIS2_PLACEMENT_3D ( 'NONE', #12344, #2406, #11192 ) ;
#9403 = DIRECTION ( 'NONE',  ( -0.000000000000000000, -0.000000000000000000, -1.000000000000000000 ) ) ;
#9404 = DIRECTION ( 'NONE',  ( 1.000000000000000000, 0.000000000000000000, 0.000000000000000000 ) ) ;
#9405 = FACE_OUTER_BOUND ( 'NONE', #5149, .T. ) ;
#9406 = ADVANCED_FACE ( 'NONE', ( #3320 ), #9064, .T. ) ;
#9407 = PLANE ( 'NONE',  #13570 ) ;
#9408 = ORIENTED_EDGE ( 'NONE', *, *, #7519, .T. ) ;
#9409 = LINE ( 'NONE', #13822, #13430 ) ;
#9410 = AXIS2_PLACEMENT_3D ( 'NONE', #8782, #7612, #10017 ) ;
#9411 = CARTESIAN_POINT ( 'NONE',  ( 137.3500000000000227, -95.00000000000008527, 186.2999999999999829 ) ) ;
#9412 = CIRCLE ( 'NONE', #1040, 1.037871761867652065 ) ;
#9413 = VERTEX_POINT ( 'NONE', #11076 ) ;
#9414 = DIRECTION ( 'NONE',  ( 0.000000000000000000, -1.000000000000000000, 0.000000000000000000 ) ) ;
#9415 = EDGE_CURVE ( 'NONE', #13552, #6403, #76, .T. ) ;
#9416 = EDGE_CURVE ( 'NONE', #145, #1188, #3973, .T. ) ;
#9417 = AXIS2_PLACEMENT_3D ( 'NONE', #5204, #14025, #4101 ) ;
#9418 = DIRECTION ( 'NONE',  ( 0.000000000000000000, 0.000000000000000000, 1.000000000000000000 ) ) ;
#9419 = EDGE_CURVE ( 'NONE', #2919, #9074, #8142, .T. ) ;
#9420 = DIRECTION ( 'NONE',  ( -1.000000000000000000, 0.000000000000000000, 0.000000000000000000 ) ) ;
#9421 = DIRECTION ( 'NONE',  ( -0.7071067811865369146, 0.000000000000000000, 0.7071067811865582309 ) ) ;
#9422 = DIRECTION ( 'NONE',  ( -0.000000000000000000, 0.000000000000000000, -1.000000000000000000 ) ) ;
#9423 = FILL_AREA_STYLE_COLOUR ( '', #4916 ) ;
#9424 = AXIS2_PLACEMENT_3D ( 'NONE', #8139, #9239, #13652 ) ;
#9425 = CARTESIAN_POINT ( 'NONE',  ( -4.236525694536558362, 2.416953475386465211, -3.751298745799836354 ) ) ;
#9426 = AXIS2_PLACEMENT_3D ( 'NONE', #3398, #13456, #11155 ) ;
#9427 = CONTEXT_DEPENDENT_SHAPE_REPRESENTATION ( #11227, #9484 ) ;
#9428 = AXIS2_PLACEMENT_3D ( 'NONE', #11423, #1466, #5902 ) ;
#9429 = ORIENTED_EDGE ( 'NONE', *, *, #10092, .F. ) ;
#9430 = AXIS2_PLACEMENT_3D ( 'NONE', #11326, #9003, #13494 ) ;
#9431 = DIRECTION ( 'NONE',  ( -1.000000000000000000, -0.000000000000000000, -0.000000000000000000 ) ) ;
#9432 = ORIENTED_EDGE ( 'NONE', *, *, #9760, .F. ) ;
#9433 = FACE_OUTER_BOUND ( 'NONE', #3209, .T. ) ;
#9434 = LINE ( 'NONE', #13845, #10902 ) ;
#9435 = VECTOR ( 'NONE', #3946, 1000.000000000000000 ) ;
#9436 = VERTEX_POINT ( 'NONE', #11350 ) ;
#9437 = LINE ( 'NONE', #5167, #6886 ) ;
#9438 = ORIENTED_EDGE ( 'NONE', *, *, #11811, .T. ) ;
#9439 = LINE ( 'NONE', #10524, #14035 ) ;
#9440 = VECTOR ( 'NONE', #12641, 1000.000000000000000 ) ;
#9441 = CARTESIAN_POINT ( 'NONE',  ( 5.000000000000004441, 0.000000000000000000, 0.000000000000000000 ) ) ;
#9442 = ORIENTED_EDGE ( 'NONE', *, *, #5442, .T. ) ;
#9443 = EDGE_CURVE ( 'NONE', #10838, #1381, #936, .T. ) ;
#9444 = FACE_BOUND ( 'NONE', #6164, .T. ) ;
#9445 = MECHANICAL_DESIGN_GEOMETRIC_PRESENTATION_REPRESENTATION (  '', ( #10851 ), #6900 ) ;
#9446 = LINE ( 'NONE', #11687, #386 ) ;
#9447 = CONICAL_SURFACE ( 'NONE', #8274, 2.500000000000000888, 0.9599310885968785900 ) ;
#9448 = DIRECTION ( 'NONE',  ( -0.000000000000000000, -0.000000000000000000, -1.000000000000000000 ) ) ;
#9449 = DIRECTION ( 'NONE',  ( -1.000000000000000000, -0.000000000000000000, -0.000000000000000000 ) ) ;
#9450 = CIRCLE ( 'NONE', #14064, 2.649999999999985700 ) ;
#9451 = ORIENTED_EDGE ( 'NONE', *, *, #11365, .F. ) ;
#9452 = ORIENTED_EDGE ( 'NONE', *, *, #2851, .T. ) ;
#9453 = DIRECTION ( 'NONE',  ( -1.000000000000000000, -0.000000000000000000, -0.000000000000000000 ) ) ;
#9454 = AXIS2_PLACEMENT_3D ( 'NONE', #8563, #4068, #8778 ) ;
#9455 = ORIENTED_EDGE ( 'NONE', *, *, #10401, .T. ) ;
#9456 = DIRECTION ( 'NONE',  ( -0.000000000000000000, 0.000000000000000000, 1.000000000000000000 ) ) ;
#9457 = ORIENTED_EDGE ( 'NONE', *, *, #12224, .T. ) ;
#9458 = FACE_OUTER_BOUND ( 'NONE', #9974, .T. ) ;
#9459 = ORIENTED_EDGE ( 'NONE', *, *, #8900, .T. ) ;
#9460 = DIRECTION ( 'NONE',  ( -0.7071067811865306973, 0.000000000000000000, 0.7071067811865643371 ) ) ;
#9461 = DIRECTION ( 'NONE',  ( 1.000000000000000000, 0.000000000000000000, 0.000000000000000000 ) ) ;
#9462 = CARTESIAN_POINT ( 'NONE',  ( -299.9999999999999432, -75.00000000000008527, 10.00000000000000178 ) ) ;
#9463 = CARTESIAN_POINT ( 'NONE',  ( 137.3500000000000227, -95.00000000000008527, -186.2999999999999829 ) ) ;
#9464 = DIRECTION ( 'NONE',  ( -0.000000000000000000, -0.000000000000000000, 1.000000000000000000 ) ) ;
#9465 = TOROIDAL_SURFACE ( 'NONE', #2043, 5.384454397937118664, 0.5155456020628804703 ) ;
#9466 = VERTEX_POINT ( 'NONE', #6051 ) ;
#9467 = ORIENTED_EDGE ( 'NONE', *, *, #12977, .T. ) ;
#9468 = ADVANCED_FACE ( 'NONE', ( #12506 ), #2644, .T. ) ;
#9469 = CARTESIAN_POINT ( 'NONE',  ( 228.6602540378443393, -90.00000000000007105, 50.00000000000001421 ) ) ;
#9470 =( REPRESENTATION_RELATIONSHIP ('NONE','NONE', #11251, #4229 ) REPRESENTATION_RELATIONSHIP_WITH_TRANSFORMATION ( #11895 )SHAPE_REPRESENTATION_RELATIONSHIP( ) );
#9471 = DIRECTION ( 'NONE',  ( -1.000000000000000000, -0.000000000000000000, -0.000000000000000000 ) ) ;
#9472 = CARTESIAN_POINT ( 'NONE',  ( 137.4999999999999716, 45.00000000000001421, 10.00000000000000000 ) ) ;
#9473 = DIRECTION ( 'NONE',  ( 1.000000000000000000, 0.000000000000000000, 0.000000000000000000 ) ) ;
#9474 = VERTEX_POINT ( 'NONE', #13512 ) ;
#9475 = VECTOR ( 'NONE', #998, 1000.000000000000000 ) ;
#9476 = FACE_BOUND ( 'NONE', #6450, .T. ) ;
#9477 = CARTESIAN_POINT ( 'NONE',  ( 434.9999999999999432, -8.660254037844389075, 200.0000000000000000 ) ) ;
#9478 = DIRECTION ( 'NONE',  ( -1.000000000000000000, 0.000000000000000000, 6.123233995736766036E-17 ) ) ;
#9479 = FACE_OUTER_BOUND ( 'NONE', #1443, .T. ) ;
#9480 = FACE_OUTER_BOUND ( 'NONE', #306, .T. ) ;
#9481 = ORIENTED_EDGE ( 'NONE', *, *, #704, .F. ) ;
#9482 = AXIS2_PLACEMENT_3D ( 'NONE', #8162, #3814, #13603 ) ;
#9483 = CARTESIAN_POINT ( 'NONE',  ( 299.9999999999999432, -75.00000000000008527, 186.2999999999999829 ) ) ;
#9484 = PRODUCT_DEFINITION_SHAPE ( 'NONE', 'NONE',  #14342 ) ;
#9485 = CARTESIAN_POINT ( 'NONE',  ( 303.3333333333333144, -25.00000000000000000, -219.8500000000001080 ) ) ;
#9486 = ORIENTED_EDGE ( 'NONE', *, *, #8012, .T. ) ;
#9488 = ADVANCED_FACE ( 'NONE', ( #4899 ), #5981, .F. ) ;
#9487 = DIRECTION ( 'NONE',  ( 0.000000000000000000, 0.000000000000000000, -1.000000000000000000 ) ) ;
#9489 =( NAMED_UNIT ( * ) SI_UNIT ( $, .STERADIAN. ) SOLID_ANGLE_UNIT ( ) );
#9490 = EDGE_CURVE ( 'NONE', #2281, #5030, #11562, .T. ) ;
#9491 = DIRECTION ( 'NONE',  ( -0.000000000000000000, -1.000000000000000000, -0.000000000000000000 ) ) ;
#9492 = AXIS2_PLACEMENT_3D ( 'NONE', #2808, #10720, #13815 ) ;
#9493 = DIRECTION ( 'NONE',  ( -0.000000000000000000, -0.000000000000000000, 1.000000000000000000 ) ) ;
#9494 = DIRECTION ( 'NONE',  ( 0.000000000000000000, 0.000000000000000000, 1.000000000000000000 ) ) ;
#9495 = CARTESIAN_POINT ( 'NONE',  ( 360.0000000000000000, 55.00000000000001421, 10.00000000000000000 ) ) ;
#9496 = CONICAL_SURFACE ( 'NONE', #1612, 2.055000000000000160, 0.7853981633974633780 ) ;
#9497 = DIRECTION ( 'NONE',  ( 0.000000000000000000, 1.000000000000000000, 0.000000000000000000 ) ) ;
#9498 = AXIS2_PLACEMENT_3D ( 'NONE', #9081, #8053, #1454 ) ;
#9499 = ITEM_DEFINED_TRANSFORMATION ( 'NONE', 'NONE', #13027,  #14039 ) ;
#9500 =( GEOMETRIC_REPRESENTATION_CONTEXT ( 3 ) GLOBAL_UNCERTAINTY_ASSIGNED_CONTEXT ( ( #9679 ) ) GLOBAL_UNIT_ASSIGNED_CONTEXT ( ( #7047, #8197, #6976 ) ) REPRESENTATION_CONTEXT ( 'NONE', 'WORKASPACE' ) );
#9501 = ORIENTED_EDGE ( 'NONE', *, *, #8070, .T. ) ;
#9502 = ADVANCED_FACE ( 'NONE', ( #4969 ), #8212, .F. ) ;
#9503 = DIRECTION ( 'NONE',  ( -1.000000000000000000, 0.000000000000000000, 0.000000000000000000 ) ) ;
#9504 = ORIENTED_EDGE ( 'NONE', *, *, #2054, .F. ) ;
#9505 = LINE ( 'NONE', #10519, #3103 ) ;
#9506 = CARTESIAN_POINT ( 'NONE',  ( 217.4999999999999147, -85.00000000000009948, -17.55500000000000327 ) ) ;
#9507 = CIRCLE ( 'NONE', #3264, 2.649999999999985700 ) ;
#9508 = ORIENTED_EDGE ( 'NONE', *, *, #5925, .T. ) ;
#9509 = LINE ( 'NONE', #2837, #6431 ) ;
#9510 = ORIENTED_EDGE ( 'NONE', *, *, #10824, .T. ) ;
#9512 = EDGE_CURVE ( 'NONE', #9107, #10453, #11390, .T. ) ;
#9511 = CARTESIAN_POINT ( 'NONE',  ( 136.6666666666666288, -14.99999999999999822, 225.1500000000000625 ) ) ;
#9513 = DIRECTION ( 'NONE',  ( 0.000000000000000000, 0.000000000000000000, -1.000000000000000000 ) ) ;
#9514 = ORIENTED_EDGE ( 'NONE', *, *, #12414, .F. ) ;
#9515 = DIRECTION ( 'NONE',  ( 0.000000000000000000, 0.4999999999999993339, -0.8660254037844390407 ) ) ;
#9516 = CIRCLE ( 'NONE', #1861, 2.649999999999985700 ) ;
#9517 = DIRECTION ( 'NONE',  ( 1.000000000000000000, 0.000000000000000000, 0.000000000000000000 ) ) ;
#9518 = DIRECTION ( 'NONE',  ( -0.000000000000000000, -0.000000000000000000, 1.000000000000000000 ) ) ;
#9519 = SHAPE_DEFINITION_REPRESENTATION ( #6576, #13104 ) ;
#9520 = DIRECTION ( 'NONE',  ( 1.000000000000000000, 0.000000000000000000, 0.000000000000000000 ) ) ;
#9521 = VECTOR ( 'NONE', #6382, 1000.000000000000000 ) ;
#9522 = ORIENTED_EDGE ( 'NONE', *, *, #2150, .T. ) ;
#9523 = ORIENTED_EDGE ( 'NONE', *, *, #7189, .T. ) ;
#9524 = ADVANCED_FACE ( 'NONE', ( #1611 ), #9388, .F. ) ;
#9525 = EDGE_CURVE ( 'NONE', #4058, #7268, #8291, .T. ) ;
#9526 = LINE ( 'NONE', #11771, #3374 ) ;
#9527 = ORIENTED_EDGE ( 'NONE', *, *, #5626, .F. ) ;
#9528 = EDGE_CURVE ( 'NONE', #11820, #8193, #13695, .T. ) ;
#9529 = DIRECTION ( 'NONE',  ( 1.000000000000000000, 0.000000000000000000, 0.000000000000000000 ) ) ;
#9530 = ORIENTED_EDGE ( 'NONE', *, *, #10621, .F. ) ;
#9531 = CARTESIAN_POINT ( 'NONE',  ( 219.9999999999999716, -25.00000000000000000, 222.5000000000000853 ) ) ;
#9532 = ORIENTED_EDGE ( 'NONE', *, *, #7087, .F. ) ;
#9533 = DIRECTION ( 'NONE',  ( 0.000000000000000000, -0.5000000000000013323, -0.8660254037844380415 ) ) ;
#9534 = EDGE_CURVE ( 'NONE', #2298, #5764, #723, .T. ) ;
#9535 = LINE ( 'NONE', #13946, #9194 ) ;
#9536 = VECTOR ( 'NONE', #7731, 1000.000000000000000 ) ;
#9537 = FACE_BOUND ( 'NONE', #7943, .T. ) ;
#9538 = APPLICATION_CONTEXT ( 'automotive_design' ) ;
#9539 = FACE_OUTER_BOUND ( 'NONE', #6458, .T. ) ;
#9540 = AXIS2_PLACEMENT_3D ( 'NONE', #5540, #9967, #11263 ) ;
#9541 =( NAMED_UNIT ( * ) SI_UNIT ( $, .STERADIAN. ) SOLID_ANGLE_UNIT ( ) );
#9542 = FACE_OUTER_BOUND ( 'NONE', #9993, .T. ) ;
#9543 = ORIENTED_EDGE ( 'NONE', *, *, #3339, .T. ) ;
#9544 = ORIENTED_EDGE ( 'NONE', *, *, #4088, .T. ) ;
#9545 = CARTESIAN_POINT ( 'NONE',  ( -4.000000000000000000, -7.806255641895631925E-15, -3.142992957459232350 ) ) ;
#9546 = CARTESIAN_POINT ( 'NONE',  ( 0.000000000000000000, 0.000000000000000000, 186.0000000000000000 ) ) ;
#9547 = DIRECTION ( 'NONE',  ( 0.000000000000000000, 0.000000000000000000, -1.000000000000000000 ) ) ;
#9548 = FACE_BOUND ( 'NONE', #11231, .T. ) ;
#9549 = VERTEX_POINT ( 'NONE', #1327 ) ;
#9550 = VECTOR ( 'NONE', #10223, 1000.000000000000000 ) ;
#9551 = DIRECTION ( 'NONE',  ( 0.000000000000000000, 0.000000000000000000, 1.000000000000000000 ) ) ;
#9552 = EDGE_CURVE ( 'NONE', #10577, #1810, #2505, .T. ) ;
#9553 = AXIS2_PLACEMENT_3D ( 'NONE', #9262, #13678, #8089 ) ;
#9554 = CARTESIAN_POINT ( 'NONE',  ( 134.5000000000000000, -75.00000000000008527, 190.0000000000000000 ) ) ;
#9555 = CARTESIAN_POINT ( 'NONE',  ( 0.000000000000000000, 0.000000000000000000, -159.9999999999999716 ) ) ;
#9556 = MECHANICAL_DESIGN_GEOMETRIC_PRESENTATION_REPRESENTATION (  '', ( #7463 ), #2847 ) ;
#9557 = LINE ( 'NONE', #2958, #1851 ) ;
#9558 = AXIS2_PLACEMENT_3D ( 'NONE', #13627, #2469, #3701 ) ;
#9559 = ORIENTED_EDGE ( 'NONE', *, *, #2621, .T. ) ;
#9560 = ORIENTED_EDGE ( 'NONE', *, *, #11029, .T. ) ;
#9561 = CARTESIAN_POINT ( 'NONE',  ( 132.3499999999999659, -36.99999999999997868, 10.00000000000000178 ) ) ;
#9562 = AXIS2_PLACEMENT_3D ( 'NONE', #7289, #5133, #1547 ) ;
#9563 = LINE ( 'NONE', #1785, #8114 ) ;
#9564 = VERTEX_POINT ( 'NONE', #3764 ) ;
#9565 = MECHANICAL_DESIGN_GEOMETRIC_PRESENTATION_REPRESENTATION (  '', ( #7009 ), #1641 ) ;
#9566 = ORIENTED_EDGE ( 'NONE', *, *, #7124, .F. ) ;
#9567 = ADVANCED_BREP_SHAPE_REPRESENTATION ( '', ( #8473, #14039 ), #4479 ) ;
#9568 = DIRECTION ( 'NONE',  ( 0.000000000000000000, -1.000000000000000000, 0.000000000000000000 ) ) ;
#9569 = EDGE_CURVE ( 'NONE', #4138, #11685, #10185, .T. ) ;
#9570 = DIRECTION ( 'NONE',  ( 1.000000000000000000, 0.000000000000000000, 0.000000000000000000 ) ) ;
#9571 = CARTESIAN_POINT ( 'NONE',  ( -3.510273485745307287, -2.827716139362669967, -3.610536846335890004 ) ) ;
#9572 = CARTESIAN_POINT ( 'NONE',  ( -294.9999999999999432, -105.0000000000000853, 40.00000000000000000 ) ) ;
#9573 =( NAMED_UNIT ( * ) SI_UNIT ( $, .STERADIAN. ) SOLID_ANGLE_UNIT ( ) );
#9574 = VECTOR ( 'NONE', #10104, 1000.000000000000000 ) ;
#9575 = CARTESIAN_POINT ( 'NONE',  ( -1.243802165048909503, 3.900692638707381921, -3.223146290109805800 ) ) ;
#9576 = CARTESIAN_POINT ( 'NONE',  ( 53.33333333333330017, -25.00000000000000000, -222.5000000000000853 ) ) ;
#9577 = ORIENTED_EDGE ( 'NONE', *, *, #1827, .T. ) ;
#9578 = EDGE_CURVE ( 'NONE', #4230, #2417, #4461, .T. ) ;
#9579 = CARTESIAN_POINT ( 'NONE',  ( 299.9999999999999432, -75.00000000000008527, 169.9999999999999716 ) ) ;
#9580 = ORIENTED_EDGE ( 'NONE', *, *, #4716, .F. ) ;
#9581 = CARTESIAN_POINT ( 'NONE',  ( 137.4999999999999432, -56.99999999999997158, -180.0000000000000000 ) ) ;
#9582 = CARTESIAN_POINT ( 'NONE',  ( -5.560781378645573980, 0.000000000000000000, -4.000000000000000000 ) ) ;
#9583 = ORIENTED_EDGE ( 'NONE', *, *, #8448, .F. ) ;
#9584 = LINE ( 'NONE', #11607, #2734 ) ;
#9585 = EDGE_LOOP ( 'NONE', ( #867, #851, #5664, #12091 ) ) ;
#9586 = PLANE ( 'NONE',  #8472 ) ;
#9587 = CYLINDRICAL_SURFACE ( 'NONE', #5259, 2.649999999999985700 ) ;
#9588 = ORIENTED_EDGE ( 'NONE', *, *, #8225, .F. ) ;
#9589 = UNCERTAINTY_MEASURE_WITH_UNIT (LENGTH_MEASURE( 1.000000000000000082E-05 ), #13225, 'distance_accuracy_value', 'NONE');
#9590 = CARTESIAN_POINT ( 'NONE',  ( 5.000000000000000888, 0.000000000000000000, 0.000000000000000000 ) ) ;
#9591 = LINE ( 'NONE', #7409, #4182 ) ;
#9592 = ITEM_DEFINED_TRANSFORMATION ( 'NONE', 'NONE', #9082,  #14039 ) ;
#9593 = DIRECTION ( 'NONE',  ( -0.000000000000000000, -0.000000000000000000, 1.000000000000000000 ) ) ;
#9594 = ORIENTED_EDGE ( 'NONE', *, *, #5946, .T. ) ;
#9595 = ORIENTED_EDGE ( 'NONE', *, *, #13449, .F. ) ;
#9596 = EDGE_CURVE ( 'NONE', #11916, #6940, #5904, .T. ) ;
#9597 = EDGE_LOOP ( 'NONE', ( #215, #4621, #6563, #8058 ) ) ;
#9598 = ADVANCED_FACE ( 'NONE', ( #4830 ), #10942, .T. ) ;
#9599 = ORIENTED_EDGE ( 'NONE', *, *, #7944, .F. ) ;
#9600 = CARTESIAN_POINT ( 'NONE',  ( 1.794155980045911036, 0.000000000000000000, 4.749999999999999112 ) ) ;
#9601 = EDGE_LOOP ( 'NONE', ( #6733, #6443 ) ) ;
#9602 = VERTEX_POINT ( 'NONE', #3213 ) ;
#9603 = DIRECTION ( 'NONE',  ( -0.000000000000000000, -0.000000000000000000, 1.000000000000000000 ) ) ;
#9604 = ORIENTED_EDGE ( 'NONE', *, *, #4391, .F. ) ;
#9605 = DIRECTION ( 'NONE',  ( 0.000000000000000000, 0.000000000000000000, 1.000000000000000000 ) ) ;
#9606 = DIRECTION ( 'NONE',  ( -0.000000000000000000, 1.000000000000000000, -0.000000000000000000 ) ) ;
#9607 = CARTESIAN_POINT ( 'NONE',  ( -30.00000000000002842, -225.0000000000000000, 169.9999999999999716 ) ) ;
#9608 = EDGE_CURVE ( 'NONE', #8094, #5470, #13940, .T. ) ;
#9609 = ADVANCED_FACE ( 'NONE', ( #9539 ), #13948, .F. ) ;
#9610 = ADVANCED_FACE ( 'NONE', ( #10548 ), #9310, .T. ) ;
#9611 = DIRECTION ( 'NONE',  ( -1.000000000000000000, 0.000000000000000000, 0.000000000000000000 ) ) ;
#9612 = CARTESIAN_POINT ( 'NONE',  ( 2.500000000000000000, -1.178949249685218303, -2.041999999999998039 ) ) ;
#9613 = PRODUCT_DEFINITION_SHAPE ( 'NONE', 'NONE',  #14353 ) ;
#9614 = AXIS2_PLACEMENT_3D ( 'NONE', #982, #4423, #5432 ) ;
#9615 = EDGE_LOOP ( 'NONE', ( #9642, #13576, #2311 ) ) ;
#9616 = ORIENTED_EDGE ( 'NONE', *, *, #5803, .F. ) ;
#9617 = CARTESIAN_POINT ( 'NONE',  ( 303.3333333333333144, -20.00000000000000000, 222.5000000000000853 ) ) ;
#9618 = DIRECTION ( 'NONE',  ( -0.000000000000000000, -0.000000000000000000, 1.000000000000000000 ) ) ;
#9619 = DIRECTION ( 'NONE',  ( 0.000000000000000000, 0.4999999999999993894, -0.8660254037844389297 ) ) ;
#9620 = AXIS2_PLACEMENT_3D ( 'NONE', #14221, #9668, #14081 ) ;
#9621 = ORIENTED_EDGE ( 'NONE', *, *, #6640, .F. ) ;
#9622 = DIRECTION ( 'NONE',  ( -0.000000000000000000, -0.000000000000000000, -1.000000000000000000 ) ) ;
#9623 = CARTESIAN_POINT ( 'NONE',  ( 219.9999999999999716, -85.00000000000007105, 55.00000000000002132 ) ) ;
#9624 = CARTESIAN_POINT ( 'NONE',  ( 299.9999999999999432, -75.00000000000008527, -190.0000000000000000 ) ) ;
#9625 = CARTESIAN_POINT ( 'NONE',  ( -30.00000000000002842, -25.00000000000000000, 169.9999999999999716 ) ) ;
#9626 = B_SPLINE_CURVE_WITH_KNOTS ( 'NONE', 3,
 ( #9906, #8298, #9545, #12868, #2874 ),
 .UNSPECIFIED., .F., .F.,
 ( 4, 1, 4 ),
 ( 0.000000000000000000, 0.002309401076758505790, 0.004618802153517011580 ),
 .UNSPECIFIED. ) ;
#9627 = ORIENTED_EDGE ( 'NONE', *, *, #5593, .F. ) ;
#9628 = AXIS2_PLACEMENT_3D ( 'NONE', #11601, #547, #4057 ) ;
#9629 = ORIENTED_EDGE ( 'NONE', *, *, #9116, .F. ) ;
#9630 = DIRECTION ( 'NONE',  ( 0.000000000000000000, 0.000000000000000000, 1.000000000000000000 ) ) ;
#9631 = EDGE_CURVE ( 'NONE', #13395, #10991, #1067, .T. ) ;
#9632 = DIRECTION ( 'NONE',  ( 0.000000000000000000, 0.000000000000000000, -1.000000000000000000 ) ) ;
#9633 = ORIENTED_EDGE ( 'NONE', *, *, #11258, .T. ) ;
#9634 = CARTESIAN_POINT ( 'NONE',  ( 140.0000000000000000, -95.00000000000008527, -190.0000000000000000 ) ) ;
#9635 = VECTOR ( 'NONE', #1511, 1000.000000000000000 ) ;
#9636 = PRODUCT_DEFINITION_CONTEXT ( 'detailed design', #7296, 'design' ) ;
#9637 = DIRECTION ( 'NONE',  ( 0.000000000000000000, 0.000000000000000000, 1.000000000000000000 ) ) ;
#9638 = TOROIDAL_SURFACE ( 'NONE', #3392, 10.20000000000000107, 0.2000000000000031197 ) ;
#9639 = CARTESIAN_POINT ( 'NONE',  ( 4.000000000000000000, -1.700175430507292473, -3.320327275037661785 ) ) ;
#9640 = DIRECTION ( 'NONE',  ( 0.000000000000000000, -1.000000000000000000, 0.000000000000000000 ) ) ;
#9641 = FILL_AREA_STYLE ('',( #11671 ) ) ;
#9642 = ORIENTED_EDGE ( 'NONE', *, *, #1428, .F. ) ;
#9643 = FACE_OUTER_BOUND ( 'NONE', #9230, .T. ) ;
#9644 = VECTOR ( 'NONE', #12388, 1000.000000000000000 ) ;
#9645 = VERTEX_POINT ( 'NONE', #6603 ) ;
#9646 = EDGE_CURVE ( 'NONE', #12598, #12063, #14282, .T. ) ;
#9647 = CARTESIAN_POINT ( 'NONE',  ( -299.9999999999999432, -95.00000000000008527, 39.99999999999997868 ) ) ;
#9648 = CARTESIAN_POINT ( 'NONE',  ( 294.4999999999999432, -95.00000000000008527, 190.0000000000000000 ) ) ;
#9649 = AXIS2_PLACEMENT_3D ( 'NONE', #1812, #637, #8411 ) ;
#9650 = EDGE_LOOP ( 'NONE', ( #4408, #632, #11252, #14155 ) ) ;
#9651 = CARTESIAN_POINT ( 'NONE',  ( -2.688821387764050996E-14, -4.618802153517012954, -0.4999999999999995559 ) ) ;
#9652 = VERTEX_POINT ( 'NONE', #6263 ) ;
#9653 = DIRECTION ( 'NONE',  ( 0.000000000000000000, -0.000000000000000000, -1.000000000000000000 ) ) ;
#9654 = DIRECTION ( 'NONE',  ( -1.000000000000000000, -0.000000000000000000, -0.000000000000000000 ) ) ;
#9655 = EDGE_LOOP ( 'NONE', ( #11778, #6749 ) ) ;
#9656 = CIRCLE ( 'NONE', #6637, 5.000000000000004441 ) ;
#9657 = DIRECTION ( 'NONE',  ( -0.000000000000000000, -1.000000000000000000, -0.000000000000000000 ) ) ;
#9658 = ADVANCED_FACE ( 'NONE', ( #8707 ), #12119, .F. ) ;
#9659 = AXIS2_PLACEMENT_3D ( 'NONE', #12236, #10062, #7736 ) ;
#9660 = CARTESIAN_POINT ( 'NONE',  ( 0.000000000000000000, 5.051668046482832750E-16, -4.000000000000000000 ) ) ;
#9661 = AXIS2_PLACEMENT_3D ( 'NONE', #1640, #6079, #7238 ) ;
#9662 = PRESENTATION_STYLE_ASSIGNMENT (( #4220 ) ) ;
#9663 = CONTEXT_DEPENDENT_SHAPE_REPRESENTATION ( #10348, #1108 ) ;
#9664 = CIRCLE ( 'NONE', #116, 2.649999999999985700 ) ;
#9665 = CARTESIAN_POINT ( 'NONE',  ( 2.740000000000000213, 0.5149999999999965716, 0.9838866223910015529 ) ) ;
#9666 = ORIENTED_EDGE ( 'NONE', *, *, #2431, .T. ) ;
#9667 = ORIENTED_EDGE ( 'NONE', *, *, #11704, .T. ) ;
#9668 = DIRECTION ( 'NONE',  ( -0.000000000000000000, 0.000000000000000000, -1.000000000000000000 ) ) ;
#9669 = AXIS2_PLACEMENT_3D ( 'NONE', #11139, #7923, #5624 ) ;
#9670 = ORIENTED_EDGE ( 'NONE', *, *, #12800, .F. ) ;
#9671 = CARTESIAN_POINT ( 'NONE',  ( 170.9999999999999716, -8.660254037844389075, 205.0000000000000284 ) ) ;
#9672 = ORIENTED_EDGE ( 'NONE', *, *, #6410, .F. ) ;
#9673 = CIRCLE ( 'NONE', #608, 5.000000000000004441 ) ;
#9674 = ORIENTED_EDGE ( 'NONE', *, *, #5525, .T. ) ;
#9675 = LINE ( 'NONE', #725, #2254 ) ;
#9676 = VERTEX_POINT ( 'NONE', #995 ) ;
#9677 = CARTESIAN_POINT ( 'NONE',  ( 219.9999999999999716, -25.00000000000000000, 219.8500000000001080 ) ) ;
#9678 = CIRCLE ( 'NONE', #9193, 5.500000000000005329 ) ;
#9679 = UNCERTAINTY_MEASURE_WITH_UNIT (LENGTH_MEASURE( 1.000000000000000082E-05 ), #7047, 'distance_accuracy_value', 'NONE');
#9680 = VECTOR ( 'NONE', #7274, 1000.000000000000000 ) ;
#9681 = FACE_OUTER_BOUND ( 'NONE', #5691, .T. ) ;
#9682 = DIRECTION ( 'NONE',  ( -0.000000000000000000, 0.000000000000000000, 1.000000000000000000 ) ) ;
#9683 = EDGE_CURVE ( 'NONE', #3582, #8038, #6194, .T. ) ;
#9684 = ADVANCED_FACE ( 'NONE', ( #8432 ), #11863, .T. ) ;
#9685 = VECTOR ( 'NONE', #13501, 1000.000000000000000 ) ;
#9686 = CARTESIAN_POINT ( 'NONE',  ( 470.0000000000000000, -20.00000000000000000, 240.0000000000000284 ) ) ;
#9687 = AXIS2_PLACEMENT_3D ( 'NONE', #2390, #4432, #13333 ) ;
#9688 = DIRECTION ( 'NONE',  ( -1.000000000000000000, 0.000000000000000000, 0.000000000000000000 ) ) ;
#9689 = ORIENTED_EDGE ( 'NONE', *, *, #2151, .T. ) ;
#9690 = VECTOR ( 'NONE', #12448, 1000.000000000000000 ) ;
#9691 = ORIENTED_EDGE ( 'NONE', *, *, #11575, .F. ) ;
#9692 = EDGE_CURVE ( 'NONE', #6551, #11920, #11402, .T. ) ;
#9693 = LINE ( 'NONE', #6351, #4933 ) ;
#9694 = ORIENTED_EDGE ( 'NONE', *, *, #6222, .T. ) ;
#9695 = CARTESIAN_POINT ( 'NONE',  ( 93.00000000000000000, 8.660254037844390851, 205.0000000000000284 ) ) ;
#9696 = DIRECTION ( 'NONE',  ( 1.000000000000000000, 0.000000000000000000, 0.000000000000000000 ) ) ;
#9697 =( GEOMETRIC_REPRESENTATION_CONTEXT ( 3 ) GLOBAL_UNCERTAINTY_ASSIGNED_CONTEXT ( ( #2864 ) ) GLOBAL_UNIT_ASSIGNED_CONTEXT ( ( #10947, #1867, #10735 ) ) REPRESENTATION_CONTEXT ( 'NONE', 'WORKASPACE' ) );
#9698 = FACE_BOUND ( 'NONE', #1348, .T. ) ;
#9699 = ORIENTED_EDGE ( 'NONE', *, *, #7150, .F. ) ;
#9700 = EDGE_CURVE ( 'NONE', #10145, #2569, #9780, .T. ) ;
#9701 = CARTESIAN_POINT ( 'NONE',  ( 53.33333333333330017, -15.00000000000000000, 225.1500000000000625 ) ) ;
#9702 = DIRECTION ( 'NONE',  ( 0.000000000000000000, 0.000000000000000000, -1.000000000000000000 ) ) ;
#9703 = CARTESIAN_POINT ( 'NONE',  ( 304.9999999999999432, 45.00000000000001421, 145.0000000000000000 ) ) ;
#9704 = DIRECTION ( 'NONE',  ( 1.000000000000000000, 0.000000000000000000, 0.000000000000000000 ) ) ;
#9705 = EDGE_LOOP ( 'NONE', ( #11622, #646, #714 ) ) ;
#9706 = ORIENTED_EDGE ( 'NONE', *, *, #6997, .T. ) ;
#9707 = EDGE_CURVE ( 'NONE', #2628, #5974, #7349, .T. ) ;
#9708 = CARTESIAN_POINT ( 'NONE',  ( -145.0000000000000284, -95.00000000000008527, 40.00000000000000000 ) ) ;
#9709 = EDGE_CURVE ( 'NONE', #7034, #12519, #11783, .T. ) ;
#9710 = CARTESIAN_POINT ( 'NONE',  ( 0.000000000000000000, 0.000000000000000000, 210.0000000000000000 ) ) ;
#9711 = PRODUCT_DEFINITION_CONTEXT ( 'detailed design', #13047, 'design' ) ;
#9712 = VERTEX_POINT ( 'NONE', #7682 ) ;
#9713 = DIRECTION ( 'NONE',  ( 1.000000000000000000, 0.000000000000000000, 0.000000000000000000 ) ) ;
#9714 = EDGE_CURVE ( 'NONE', #7984, #1244, #9809, .T. ) ;
#9715 = DIRECTION ( 'NONE',  ( 0.000000000000000000, -0.000000000000000000, -1.000000000000000000 ) ) ;
#9716 = CIRCLE ( 'NONE', #6226, 0.2000000000000022593 ) ;
#9717 = DIRECTION ( 'NONE',  ( -0.000000000000000000, -0.000000000000000000, -1.000000000000000000 ) ) ;
#9718 = DIRECTION ( 'NONE',  ( -0.000000000000000000, 0.000000000000000000, -1.000000000000000000 ) ) ;
#9719 = CARTESIAN_POINT ( 'NONE',  ( 0.000000000000000000, 0.000000000000000000, 0.000000000000000000 ) ) ;
#9720 = CONTEXT_DEPENDENT_SHAPE_REPRESENTATION ( #13719, #7280 ) ;
#9721 = VERTEX_POINT ( 'NONE', #8781 ) ;
#9722 = CARTESIAN_POINT ( 'NONE',  ( -30.00000000000000000, 0.000000000000000000, 205.0000000000000284 ) ) ;
#9723 = ORIENTED_EDGE ( 'NONE', *, *, #5778, .T. ) ;
#9724 = DIRECTION ( 'NONE',  ( -1.000000000000000000, -0.000000000000000000, -0.000000000000000000 ) ) ;
#9725 = DIRECTION ( 'NONE',  ( -1.000000000000000000, 0.000000000000000000, -0.000000000000000000 ) ) ;
#9726 = ORIENTED_EDGE ( 'NONE', *, *, #3318, .T. ) ;
#9727 = CARTESIAN_POINT ( 'NONE',  ( 2.500000000000000000, 2.357898499370433054, -1.951563910473907981E-15 ) ) ;
#9728 = ORIENTED_EDGE ( 'NONE', *, *, #8296, .F. ) ;
#9729 = AXIS2_PLACEMENT_3D ( 'NONE', #2591, #5776, #3604 ) ;
#9730 = CARTESIAN_POINT ( 'NONE',  ( 0.000000000000000000, 0.000000000000000000, 0.000000000000000000 ) ) ;
#9731 = CARTESIAN_POINT ( 'NONE',  ( -4.000000000000000888, 1.563622288139195238, -0.2253451193528307472 ) ) ;
#9732 = VERTEX_POINT ( 'NONE', #4435 ) ;
#9733 = FACE_OUTER_BOUND ( 'NONE', #10616, .T. ) ;
#9734 = CYLINDRICAL_SURFACE ( 'NONE', #14187, 2.649999999999985700 ) ;
#9735 = EDGE_CURVE ( 'NONE', #5871, #11569, #13251, .T. ) ;
#9736 = FACE_OUTER_BOUND ( 'NONE', #11861, .T. ) ;
#9737 = CONTEXT_DEPENDENT_SHAPE_REPRESENTATION ( #8027, #2647 ) ;
#9738 = CARTESIAN_POINT ( 'NONE',  ( -4.197312064133472020, -0.8182229787990021874, -3.502518405183886685 ) ) ;
#9739 = VERTEX_POINT ( 'NONE', #5046 ) ;
#9740 = VERTEX_POINT ( 'NONE', #6122 ) ;
#9741 = PLANE ( 'NONE',  #1720 ) ;
#9742 = VERTEX_POINT ( 'NONE', #9463 ) ;
#9743 = CONICAL_SURFACE ( 'NONE', #3707, 2.059999999999998721, 0.9599310885968738161 ) ;
#9744 = CARTESIAN_POINT ( 'NONE',  ( 299.9999999999999432, -95.00000000000008527, 190.0000000000000000 ) ) ;
#9745 = ORIENTED_EDGE ( 'NONE', *, *, #13389, .F. ) ;
#9746 = AXIS2_PLACEMENT_3D ( 'NONE', #2032, #10531, #1738 ) ;
#9747 = ORIENTED_EDGE ( 'NONE', *, *, #5351, .T. ) ;
#9748 = PLANE ( 'NONE',  #12439 ) ;
#9749 = ORIENTED_EDGE ( 'NONE', *, *, #10861, .F. ) ;
#9750 = CARTESIAN_POINT ( 'NONE',  ( 0.06760930072668894231, -0.9010842325122929708, -0.5150000000000000133 ) ) ;
#9751 = FACE_OUTER_BOUND ( 'NONE', #1822, .T. ) ;
#9752 = DIRECTION ( 'NONE',  ( -0.000000000000000000, -0.000000000000000000, -1.000000000000000000 ) ) ;
#9753 = AXIS2_PLACEMENT_3D ( 'NONE', #8388, #5924, #13824 ) ;
#9754 =( REPRESENTATION_RELATIONSHIP ('NONE','NONE', #11251, #7730 ) REPRESENTATION_RELATIONSHIP_WITH_TRANSFORMATION ( #1647 )SHAPE_REPRESENTATION_RELATIONSHIP( ) );
#9755 = DIRECTION ( 'NONE',  ( 1.000000000000000000, 0.000000000000000000, 0.000000000000000000 ) ) ;
#9756 = CARTESIAN_POINT ( 'NONE',  ( 79.99999999999971578, 35.00000000000000000, 10.00000000000000000 ) ) ;
#9757 = ORIENTED_EDGE ( 'NONE', *, *, #11621, .T. ) ;
#9758 = VECTOR ( 'NONE', #6153, 1000.000000000000114 ) ;
#9759 = EDGE_LOOP ( 'NONE', ( #9170, #364, #3428, #5373 ) ) ;
#9760 = EDGE_CURVE ( 'NONE', #1149, #12343, #13874, .T. ) ;
#9761 = CARTESIAN_POINT ( 'NONE',  ( -140.0000000000000000, -95.00000000000008527, -14.14213562373090127 ) ) ;
#9762 = EDGE_CURVE ( 'NONE', #7321, #4963, #6995, .T. ) ;
#9763 = AXIS2_PLACEMENT_3D ( 'NONE', #2294, #6718, #12158 ) ;
#9764 = ORIENTED_EDGE ( 'NONE', *, *, #4909, .T. ) ;
#9765 = CARTESIAN_POINT ( 'NONE',  ( -297.4999999999999432, -75.00000000000008527, 0.000000000000000000 ) ) ;
#9766 = FACE_OUTER_BOUND ( 'NONE', #1344, .T. ) ;
#9767 = CARTESIAN_POINT ( 'NONE',  ( -30.00000000000002842, -20.00000000000000000, 240.0000000000000284 ) ) ;
#9768 = ORIENTED_EDGE ( 'NONE', *, *, #8317, .T. ) ;
#9769 = FACE_OUTER_BOUND ( 'NONE', #4424, .T. ) ;
#9770 = DIRECTION ( 'NONE',  ( -0.000000000000000000, -0.000000000000000000, 1.000000000000000000 ) ) ;
#9771 = AXIS2_PLACEMENT_3D ( 'NONE', #7721, #1104, #13305 ) ;
#9772 = LINE ( 'NONE', #11145, #8325 ) ;
#9773 = VERTEX_POINT ( 'NONE', #4572 ) ;
#9774 = ORIENTED_EDGE ( 'NONE', *, *, #10592, .F. ) ;
#9775 = EDGE_CURVE ( 'NONE', #931, #4036, #1307, .T. ) ;
#9776 = CARTESIAN_POINT ( 'NONE',  ( 137.4999999999999432, -36.99999999999997868, -180.0000000000000000 ) ) ;
#9777 = EDGE_CURVE ( 'NONE', #9466, #4042, #1359, .T. ) ;
#9778 = SHAPE_REPRESENTATION ( 'aligner', ( #14039 ), #4479 ) ;
#9779 = PLANE ( 'NONE',  #13226 ) ;
#9780 = CIRCLE ( 'NONE', #2134, 5.500000000000005329 ) ;
#9781 = B_SPLINE_CURVE_WITH_KNOTS ( 'NONE', 3,
 ( #10870, #11954, #10797, #11807 ),
 .UNSPECIFIED., .F., .F.,
 ( 4, 4 ),
 ( 0.004656695506220393486, 0.007337072593346776264 ),
 .UNSPECIFIED. ) ;
#9782 = ORIENTED_EDGE ( 'NONE', *, *, #12092, .T. ) ;
#9783 = CARTESIAN_POINT ( 'NONE',  ( 0.000000000000000000, 2.357898499370433054, -1.951563910473907981E-15 ) ) ;
#9784 = AXIS2_PLACEMENT_3D ( 'NONE', #1045, #3470, #2303 ) ;
#9785 = CARTESIAN_POINT ( 'NONE',  ( 93.00000000000000000, -8.660254037844389075, 200.0000000000000000 ) ) ;
#9786 = AXIS2_PLACEMENT_3D ( 'NONE', #7762, #4299, #10833 ) ;
#9787 = ADVANCED_FACE ( 'NONE', ( #3487 ), #10466, .F. ) ;
#9788 = EDGE_CURVE ( 'NONE', #5508, #328, #1281, .T. ) ;
#9789 = CARTESIAN_POINT ( 'NONE',  ( 140.0000000000000000, -95.00000000000008527, 190.0000000000000000 ) ) ;
#9790 = EDGE_CURVE ( 'NONE', #9959, #2372, #2535, .T. ) ;
#9791 = ITEM_DEFINED_TRANSFORMATION ( 'NONE', 'NONE', #6077,  #14039 ) ;
#9792 = ORIENTED_EDGE ( 'NONE', *, *, #8225, .T. ) ;
#9793 = CARTESIAN_POINT ( 'NONE',  ( 4.999999999999999112, 8.660254037844390851, 205.0000000000000284 ) ) ;
#9794 = AXIS2_PLACEMENT_3D ( 'NONE', #3679, #6934, #9039 ) ;
#9795 =( GEOMETRIC_REPRESENTATION_CONTEXT ( 3 ) GLOBAL_UNCERTAINTY_ASSIGNED_CONTEXT ( ( #5390 ) ) GLOBAL_UNIT_ASSIGNED_CONTEXT ( ( #2971, #8239, #12674 ) ) REPRESENTATION_CONTEXT ( 'NONE', 'WORKASPACE' ) );
#9796 = ORIENTED_EDGE ( 'NONE', *, *, #11653, .T. ) ;
#9797 = LINE ( 'NONE', #14202, #10203 ) ;
#9798 = CARTESIAN_POINT ( 'NONE',  ( -30.00000000000002842, -225.0000000000000000, 190.0000000000000000 ) ) ;
#9799 = ORIENTED_EDGE ( 'NONE', *, *, #4387, .F. ) ;
#9800 = ORIENTED_EDGE ( 'NONE', *, *, #7894, .T. ) ;
#9801 = CARTESIAN_POINT ( 'NONE',  ( -31.74999999999995737, 3.061616997868383634E-16, -2.500000000000000444 ) ) ;
#9802 = CARTESIAN_POINT ( 'NONE',  ( 304.9999999999999432, 45.00000000000001421, 10.00000000000000000 ) ) ;
#9805 = ORIENTED_EDGE ( 'NONE', *, *, #10934, .T. ) ;
#9804 = AXIS2_PLACEMENT_3D ( 'NONE', #8273, #13926, #2769 ) ;
#9803 = AXIS2_PLACEMENT_3D ( 'NONE', #879, #12807, #3448 ) ;
#9806 = CARTESIAN_POINT ( 'NONE',  ( 302.6499999999999204, -75.00000000000008527, -169.9999999999999716 ) ) ;
#9807 = DIRECTION ( 'NONE',  ( 0.000000000000000000, 1.000000000000000000, 0.000000000000000000 ) ) ;
#9808 = PRODUCT_DEFINITION_FORMATION_WITH_SPECIFIED_SOURCE ( 'ANY', '', #3229, .NOT_KNOWN. ) ;
#9809 = LINE ( 'NONE', #5444, #5156 ) ;
#9810 = CARTESIAN_POINT ( 'NONE',  ( 0.000000000000000000, 0.000000000000000000, -4.974599999999998801 ) ) ;
#9811 = DIRECTION ( 'NONE',  ( -0.000000000000000000, -0.000000000000000000, -1.000000000000000000 ) ) ;
#9812 = ORIENTED_EDGE ( 'NONE', *, *, #3673, .T. ) ;
#9813 = ORIENTED_EDGE ( 'NONE', *, *, #12163, .T. ) ;
#9814 = DIRECTION ( 'NONE',  ( 1.000000000000000000, 0.000000000000000000, 0.000000000000000000 ) ) ;
#9815 = ORIENTED_EDGE ( 'NONE', *, *, #1803, .T. ) ;
#9816 = CARTESIAN_POINT ( 'NONE',  ( -124.9999999999999432, -105.0000000000000853, 30.00000000000000000 ) ) ;
#9817 = ORIENTED_EDGE ( 'NONE', *, *, #6199, .T. ) ;
#9818 = EDGE_CURVE ( 'NONE', #3380, #1127, #11384, .T. ) ;
#9819 = EDGE_LOOP ( 'NONE', ( #7131, #11003 ) ) ;
#9820 = CARTESIAN_POINT ( 'NONE',  ( 1.424271237134740131, 0.000000000000000000, 0.000000000000000000 ) ) ;
#9821 = ORIENTED_EDGE ( 'NONE', *, *, #14193, .F. ) ;
#9822 = DIRECTION ( 'NONE',  ( -0.000000000000000000, 0.000000000000000000, 1.000000000000000000 ) ) ;
#9823 = DIRECTION ( 'NONE',  ( 0.000000000000000000, 1.000000000000000000, 0.000000000000000000 ) ) ;
#9824 = FACE_OUTER_BOUND ( 'NONE', #14298, .T. ) ;
#9825 = DIRECTION ( 'NONE',  ( 0.000000000000000000, 1.224646799147351975E-16, 1.000000000000000000 ) ) ;
#9826 =( NAMED_UNIT ( * ) PLANE_ANGLE_UNIT ( ) SI_UNIT ( $, .RADIAN. ) );
#9827 = DIRECTION ( 'NONE',  ( 1.000000000000000000, 0.000000000000000000, 0.000000000000000000 ) ) ;
#9828 = EDGE_LOOP ( 'NONE', ( #9092, #6869, #5117, #12012 ) ) ;
#9829 = VERTEX_POINT ( 'NONE', #5867 ) ;
#9830 = CARTESIAN_POINT ( 'NONE',  ( 53.33333333333330017, -20.00000000000000000, 222.5000000000000853 ) ) ;
#9831 = ORIENTED_EDGE ( 'NONE', *, *, #4716, .T. ) ;
#9832 = CARTESIAN_POINT ( 'NONE',  ( 2.500000000000000000, -1.178949249685213863, 2.042000000000002924 ) ) ;
#9833 = DIRECTION ( 'NONE',  ( 1.000000000000000000, 0.000000000000000000, -0.000000000000000000 ) ) ;
#9834 = FACE_BOUND ( 'NONE', #2082, .T. ) ;
#9835 = B_SPLINE_CURVE_WITH_KNOTS ( 'NONE', 3,
 ( #12988, #771, #1657, #6098, #3921, #7254 ),
 .UNSPECIFIED., .F., .F.,
 ( 4, 2, 4 ),
 ( 0.002452478801916376308, 0.003676905084148007850, 0.004901331366379639391 ),
 .UNSPECIFIED. ) ;
#9836 = EDGE_LOOP ( 'NONE', ( #4635, #10901 ) ) ;
#9837 = CARTESIAN_POINT ( 'NONE',  ( 297.3499999999999659, -95.00000000000008527, -190.0000000000000000 ) ) ;
#9838 = EDGE_CURVE ( 'NONE', #10809, #12252, #6065, .T. ) ;
#9839 = DIRECTION ( 'NONE',  ( 1.000000000000000000, 0.000000000000000000, 0.000000000000000000 ) ) ;
#9840 = DIRECTION ( 'NONE',  ( 6.123233995736766036E-17, 0.000000000000000000, 1.000000000000000000 ) ) ;
#9841 = FACE_OUTER_BOUND ( 'NONE', #8537, .T. ) ;
#9842 = ORIENTED_EDGE ( 'NONE', *, *, #504, .F. ) ;
#9843 = EDGE_LOOP ( 'NONE', ( #4019, #11712, #265, #12536 ) ) ;
#9844 = CARTESIAN_POINT ( 'NONE',  ( -30.00000000000002842, -20.00000000000000000, -250.0000000000000000 ) ) ;
#9845 = PRODUCT_DEFINITION_SHAPE ( 'NONE', 'NONE',  #14360 ) ;
#9846 = CARTESIAN_POINT ( 'NONE',  ( 119.9999999999999147, -20.00000000000000000, 169.9999999999999716 ) ) ;
#9847 = ORIENTED_EDGE ( 'NONE', *, *, #12447, .T. ) ;
#9848 = CARTESIAN_POINT ( 'NONE',  ( 2.500000000000000000, -2.357898499370432610, 3.252606517456513302E-15 ) ) ;
#9849 = FACE_OUTER_BOUND ( 'NONE', #6452, .T. ) ;
#9850 = EDGE_CURVE ( 'NONE', #2351, #11069, #10707, .T. ) ;
#9851 = CARTESIAN_POINT ( 'NONE',  ( 0.000000000000000000, 1.178949249685213863, -2.042000000000001148 ) ) ;
#9852 = CARTESIAN_POINT ( 'NONE',  ( 219.9999999999999716, -30.00000000000000355, 222.5000000000000853 ) ) ;
#9853 = AXIS2_PLACEMENT_3D ( 'NONE', #6470, #12191, #11987 ) ;
#9854 = AXIS2_PLACEMENT_3D ( 'NONE', #11197, #14231, #14189 ) ;
#9855 = EDGE_LOOP ( 'NONE', ( #11191, #3004, #7423, #13549 ) ) ;
#9856 = DIRECTION ( 'NONE',  ( 1.000000000000000000, 0.000000000000000000, 0.000000000000000000 ) ) ;
#9857 = ORIENTED_EDGE ( 'NONE', *, *, #11588, .T. ) ;
#9858 = CARTESIAN_POINT ( 'NONE',  ( -0.02448733951239248641, -4.877042772274742255, -3.751161874094027571 ) ) ;
#9859 = DIRECTION ( 'NONE',  ( -1.000000000000000000, 0.000000000000000000, 0.000000000000000000 ) ) ;
#9860 = ADVANCED_FACE ( 'NONE', ( #12327 ), #13538, .F. ) ;
#9861 = EDGE_CURVE ( 'NONE', #7098, #6551, #2320, .T. ) ;
#9862 = AXIS2_PLACEMENT_3D ( 'NONE', #1907, #8725, #4160 ) ;
#9863 = CIRCLE ( 'NONE', #14252, 2.649999999999985700 ) ;
#9864 = ORIENTED_EDGE ( 'NONE', *, *, #2443, .T. ) ;
#9865 = EDGE_CURVE ( 'NONE', #1020, #12884, #13406, .T. ) ;
#9866 = VERTEX_POINT ( 'NONE', #7824 ) ;
#9867 = LINE ( 'NONE', #4358, #586 ) ;
#9868 = UNCERTAINTY_MEASURE_WITH_UNIT (LENGTH_MEASURE( 1.000000000000000082E-05 ), #5519, 'distance_accuracy_value', 'NONE');
#9869 = CARTESIAN_POINT ( 'NONE',  ( -4.140404888673278272, -2.228338276487456415, -3.686887068327035166 ) ) ;
#9870 = DIRECTION ( 'NONE',  ( -0.000000000000000000, 0.000000000000000000, 1.000000000000000000 ) ) ;
#9871 = CARTESIAN_POINT ( 'NONE',  ( 305.0000000000000000, -36.99999999999997868, -180.0000000000000000 ) ) ;
#9872 = FACE_OUTER_BOUND ( 'NONE', #6965, .T. ) ;
#9873 = CARTESIAN_POINT ( 'NONE',  ( 299.9999999999999432, -95.00000000000008527, 186.2999999999999829 ) ) ;
#9874 = CARTESIAN_POINT ( 'NONE',  ( -4.000000000000000000, -0.8382240730041925492, -3.220610619767135141 ) ) ;
#9875 = AXIS2_PLACEMENT_3D ( 'NONE', #8100, #3613, #9351 ) ;
#9876 = ORIENTED_EDGE ( 'NONE', *, *, #1399, .F. ) ;
#9877 = ORIENTED_EDGE ( 'NONE', *, *, #12521, .F. ) ;
#9878 = AXIS2_PLACEMENT_3D ( 'NONE', #5234, #9654, #7475 ) ;
#9879 = DIRECTION ( 'NONE',  ( -0.000000000000000000, 1.000000000000000000, -0.000000000000000000 ) ) ;
#9880 = EDGE_LOOP ( 'NONE', ( #4673, #7981 ) ) ;
#9881 = DIRECTION ( 'NONE',  ( -0.000000000000000000, -0.000000000000000000, -1.000000000000000000 ) ) ;
#9882 = ORIENTED_EDGE ( 'NONE', *, *, #8258, .T. ) ;
#9883 = EDGE_CURVE ( 'NONE', #14268, #1244, #7220, .T. ) ;
#9884 = ORIENTED_EDGE ( 'NONE', *, *, #7442, .F. ) ;
#9885 = LINE ( 'NONE', #12197, #1543 ) ;
#9886 = EDGE_LOOP ( 'NONE', ( #12408, #3529, #12840, #12139 ) ) ;
#9887 = CARTESIAN_POINT ( 'NONE',  ( 142.6500000000000057, -95.00000000000008527, 186.2999999999999829 ) ) ;
#9888 = VECTOR ( 'NONE', #1789, 1000.000000000000000 ) ;
#9889 = CARTESIAN_POINT ( 'NONE',  ( 3.999999999999999112, -1.539600717839012978, -3.300726591567080703 ) ) ;
#9890 = DIRECTION ( 'NONE',  ( -1.000000000000000000, -0.000000000000000000, -0.000000000000000000 ) ) ;
#9891 = ADVANCED_FACE ( 'NONE', ( #46 ), #12393, .T. ) ;
#9892 = CIRCLE ( 'NONE', #354, 5.000000000000004441 ) ;
#9893 = DIRECTION ( 'NONE',  ( -1.000000000000000000, -0.000000000000000000, -0.000000000000000000 ) ) ;
#9894 =( NAMED_UNIT ( * ) PLANE_ANGLE_UNIT ( ) SI_UNIT ( $, .RADIAN. ) );
#9895 = CARTESIAN_POINT ( 'NONE',  ( 137.3500000000000227, -75.00000000000008527, 186.2999999999999829 ) ) ;
#9896 = AXIS2_PLACEMENT_3D ( 'NONE', #1249, #3587, #147 ) ;
#9897 = EDGE_LOOP ( 'NONE', ( #9588, #4960 ) ) ;
#9898 = CIRCLE ( 'NONE', #10115, 2.649999999999985700 ) ;
#9899 = ORIENTED_EDGE ( 'NONE', *, *, #1597, .T. ) ;
#9900 = AXIS2_PLACEMENT_3D ( 'NONE', #6171, #2629, #2843 ) ;
#9902 = LINE ( 'NONE', #5680, #9574 ) ;
#9901 = VECTOR ( 'NONE', #13008, 1000.000000000000000 ) ;
#9903 = VECTOR ( 'NONE', #13993, 1000.000000000000000 ) ;
#9904 = EDGE_LOOP ( 'NONE', ( #5523, #10852, #2853, #7219 ) ) ;
#9905 = DIRECTION ( 'NONE',  ( 1.000000000000000000, 0.000000000000000000, 0.000000000000000000 ) ) ;
#9906 = CARTESIAN_POINT ( 'NONE',  ( -4.000000000000000000, 2.309401076758498483, -3.433295621305379353 ) ) ;
#9907 = DIRECTION ( 'NONE',  ( 0.000000000000000000, 0.000000000000000000, 1.000000000000000000 ) ) ;
#9908 = VECTOR ( 'NONE', #2131, 1000.000000000000000 ) ;
#9909 = ORIENTED_EDGE ( 'NONE', *, *, #3196, .T. ) ;
#9910 = CIRCLE ( 'NONE', #9454, 5.500000000000005329 ) ;
#9911 = DIRECTION ( 'NONE',  ( 0.000000000000000000, 0.000000000000000000, 1.000000000000000000 ) ) ;
#9912 = CIRCLE ( 'NONE', #5726, 5.500000000000005329 ) ;
#9913 = CARTESIAN_POINT ( 'NONE',  ( 2.100000000000000089, 0.000000000000000000, -0.2800830152838844622 ) ) ;
#9914 = AXIS2_PLACEMENT_3D ( 'NONE', #2604, #13472, #463 ) ;
#9915 = DIRECTION ( 'NONE',  ( -1.000000000000000000, 0.000000000000000000, 0.000000000000000000 ) ) ;
#9916 = ADVANCED_FACE ( 'NONE', ( #13475 ), #4783, .F. ) ;
#9917 = ORIENTED_EDGE ( 'NONE', *, *, #5694, .F. ) ;
#9918 = FACE_OUTER_BOUND ( 'NONE', #10891, .T. ) ;
#9919 = AXIS2_PLACEMENT_3D ( 'NONE', #6225, #5152, #9637 ) ;
#9920 = DIRECTION ( 'NONE',  ( 0.000000000000000000, 0.000000000000000000, 1.000000000000000000 ) ) ;
#9921 = VECTOR ( 'NONE', #3521, 1000.000000000000000 ) ;
#9922 = ORIENTED_EDGE ( 'NONE', *, *, #8875, .F. ) ;
#9923 = CARTESIAN_POINT ( 'NONE',  ( -314.9999999999999432, -105.0000000000000995, 40.00000000000000000 ) ) ;
#9924 = CARTESIAN_POINT ( 'NONE',  ( -5.000000000000000888, 8.660254037844390851, 199.9990000000000236 ) ) ;
#9925 = CYLINDRICAL_SURFACE ( 'NONE', #5769, 2.649999999999985700 ) ;
#9926 = CARTESIAN_POINT ( 'NONE',  ( 136.6666666666666288, -30.00000000000000355, 222.5000000000000853 ) ) ;
#9927 = ITEM_DEFINED_TRANSFORMATION ( 'NONE', 'NONE', #6541,  #14039 ) ;
#9928 = VECTOR ( 'NONE', #4406, 1000.000000000000000 ) ;
#9929 = ORIENTED_EDGE ( 'NONE', *, *, #12338, .T. ) ;
#9930 = LINE ( 'NONE', #7701, #2442 ) ;
#9931 = PRODUCT_DEFINITION_SHAPE ( 'NONE', 'NONE',  #14318 ) ;
#9932 = ORIENTED_EDGE ( 'NONE', *, *, #5887, .T. ) ;
#9933 = CARTESIAN_POINT ( 'NONE',  ( 0.000000000000000000, 0.000000000000000000, 200.0000000000000000 ) ) ;
#9934 = FACE_OUTER_BOUND ( 'NONE', #6514, .T. ) ;
#9935 = EDGE_CURVE ( 'NONE', #3017, #1918, #3421, .T. ) ;
#9936 = EDGE_CURVE ( 'NONE', #8189, #7589, #107, .T. ) ;
#9937 =( REPRESENTATION_RELATIONSHIP ('NONE','NONE', #11251, #208 ) REPRESENTATION_RELATIONSHIP_WITH_TRANSFORMATION ( #8417 )SHAPE_REPRESENTATION_RELATIONSHIP( ) );
#9938 = VERTEX_POINT ( 'NONE', #2749 ) ;
#9939 = EDGE_LOOP ( 'NONE', ( #14083, #2579, #11935, #7044 ) ) ;
#9941 = CIRCLE ( 'NONE', #3680, 2.500000000000002220 ) ;
#9940 = CARTESIAN_POINT ( 'NONE',  ( 13.50000000000000000, 1.653273178848926867E-15, -190.0000000000000000 ) ) ;
#9942 = DIRECTION ( 'NONE',  ( 0.000000000000000000, 0.000000000000000000, -1.000000000000000000 ) ) ;
#9943 = SURFACE_STYLE_FILL_AREA ( #12467 ) ;
#9944 = CIRCLE ( 'NONE', #8548, 2.649999999999985700 ) ;
#9945 = DIRECTION ( 'NONE',  ( -1.000000000000000000, -0.000000000000000000, -0.000000000000000000 ) ) ;
#9946 = DIRECTION ( 'NONE',  ( -0.000000000000000000, 1.000000000000000000, -0.000000000000000000 ) ) ;
#9947 = FACE_OUTER_BOUND ( 'NONE', #2706, .T. ) ;
#9948 = DIRECTION ( 'NONE',  ( 0.000000000000000000, 1.000000000000000000, 0.000000000000000000 ) ) ;
#9949 = EDGE_CURVE ( 'NONE', #3581, #3491, #10004, .T. ) ;
#9950 = DIRECTION ( 'NONE',  ( -1.000000000000000000, -0.000000000000000000, -0.000000000000000000 ) ) ;
#9951 = EDGE_LOOP ( 'NONE', ( #4180, #7435 ) ) ;
#9952 = ORIENTED_EDGE ( 'NONE', *, *, #13309, .F. ) ;
#9953 = DIRECTION ( 'NONE',  ( -1.000000000000000000, -0.000000000000000000, -0.000000000000000000 ) ) ;
#9954 = ORIENTED_EDGE ( 'NONE', *, *, #5126, .T. ) ;
#9955 = PLANE ( 'NONE',  #7227 ) ;
#9956 = VECTOR ( 'NONE', #7224, 1000.000000000000000 ) ;
#9957 = EDGE_CURVE ( 'NONE', #3293, #3594, #3833, .T. ) ;
#9958 = EDGE_CURVE ( 'NONE', #1312, #9004, #1435, .T. ) ;
#9959 = VERTEX_POINT ( 'NONE', #11451 ) ;
#9960 = LINE ( 'NONE', #6692, #5957 ) ;
#9961 = ORIENTED_EDGE ( 'NONE', *, *, #6248, .F. ) ;
#9962 = VECTOR ( 'NONE', #1109, 1000.000000000000000 ) ;
#9963 = CARTESIAN_POINT ( 'NONE',  ( -299.9999999999999432, -75.00000000000008527, 39.99999999999997868 ) ) ;
#9964 = CARTESIAN_POINT ( 'NONE',  ( 4.000000000000000000, -2.309401076758516691, -0.4999999999999995559 ) ) ;
#9965 = EDGE_CURVE ( 'NONE', #1964, #3920, #10583, .T. ) ;
#9966 = CARTESIAN_POINT ( 'NONE',  ( 0.2500000000000002220, 0.000000000000000000, 0.000000000000000000 ) ) ;
#9967 = DIRECTION ( 'NONE',  ( 1.000000000000000000, 0.000000000000000000, 0.000000000000000000 ) ) ;
#9968 = EDGE_CURVE ( 'NONE', #8495, #10689, #10511, .T. ) ;
#9969 = EDGE_CURVE ( 'NONE', #9712, #3954, #12543, .T. ) ;
#9970 = DIRECTION ( 'NONE',  ( 1.000000000000000000, 0.000000000000000000, 0.000000000000000000 ) ) ;
#9971 = ORIENTED_EDGE ( 'NONE', *, *, #12798, .F. ) ;
#9972 = EDGE_CURVE ( 'NONE', #1006, #8809, #1568, .T. ) ;
#9973 = EDGE_CURVE ( 'NONE', #50, #7761, #12680, .T. ) ;
#9974 = EDGE_LOOP ( 'NONE', ( #5391, #13918, #6341, #6063 ) ) ;
#9975 = AXIS2_PLACEMENT_3D ( 'NONE', #13357, #2198, #4595 ) ;
#9976 = ADVANCED_FACE ( 'NONE', ( #9278 ), #8395, .T. ) ;
#9977 = CARTESIAN_POINT ( 'NONE',  ( 181.0000000000000000, -8.660254037844389075, 200.0000000000000000 ) ) ;
#9978 = EDGE_LOOP ( 'NONE', ( #6020, #13268, #8570, #4080 ) ) ;
#9979 = DIRECTION ( 'NONE',  ( 0.000000000000000000, 0.000000000000000000, 1.000000000000000000 ) ) ;
#9980 = DIRECTION ( 'NONE',  ( 0.000000000000000000, 0.000000000000000000, -1.000000000000000000 ) ) ;
#9981 = LINE ( 'NONE', #1183, #8758 ) ;
#9982 = ORIENTED_EDGE ( 'NONE', *, *, #6482, .T. ) ;
#9983 = CARTESIAN_POINT ( 'NONE',  ( 5.000000000000002665, 0.000000000000000000, -2.700000000000000622 ) ) ;
#9984 = CARTESIAN_POINT ( 'NONE',  ( 132.3499999999999659, -36.99999999999997868, 0.000000000000000000 ) ) ;
#9985 = PLANE ( 'NONE',  #669 ) ;
#9986 = CARTESIAN_POINT ( 'NONE',  ( -4.101948962586059899, -2.368261337751176754, -3.681124513963741851 ) ) ;
#9987 = VERTEX_POINT ( 'NONE', #466 ) ;
#9988 = CYLINDRICAL_SURFACE ( 'NONE', #2561, 2.500000000000002220 ) ;
#9989 = CIRCLE ( 'NONE', #4204, 0.2000000000000000944 ) ;
#9990 = CARTESIAN_POINT ( 'NONE',  ( -144.9999999999999432, -65.00000000000008527, 40.00000000000000000 ) ) ;
#9991 = CARTESIAN_POINT ( 'NONE',  ( 0.000000000000000000, 0.000000000000000000, 0.000000000000000000 ) ) ;
#9992 = EDGE_CURVE ( 'NONE', #13397, #532, #7163, .T. ) ;
#9993 = EDGE_LOOP ( 'NONE', ( #13635, #10553, #2446, #875, #10765 ) ) ;
#9994 = CARTESIAN_POINT ( 'NONE',  ( 4.000000000000000000, -2.309401076758516691, -0.4999999999999995559 ) ) ;
#9995 = CONICAL_SURFACE ( 'NONE', #10458, 2.500000000000002220, 1.029744260000002631 ) ;
#9996 = CARTESIAN_POINT ( 'NONE',  ( 0.000000000000000000, 0.000000000000000000, 0.000000000000000000 ) ) ;
#9997 = COLOUR_RGB ( '',0.8941176470588234615, 0.8941176470588234615, 0.8941176470588234615 ) ;
#9998 = LINE ( 'NONE', #12312, #11121 ) ;
#9999 = DIRECTION ( 'NONE',  ( 6.123233995736766036E-17, -1.000000000000000000, 0.000000000000000000 ) ) ;
#10000=STYLED_ITEM('',(#14396),#3823);
#10001 = ITEM_DEFINED_TRANSFORMATION ( 'NONE', 'NONE', #14176,  #14039 ) ;
#10002 = ORIENTED_EDGE ( 'NONE', *, *, #1882, .F. ) ;
#10003 = DIRECTION ( 'NONE',  ( 0.000000000000000000, 0.000000000000000000, 1.000000000000000000 ) ) ;
#10004 = CIRCLE ( 'NONE', #3744, 12.00000000000000000 ) ;
#10005 = ORIENTED_EDGE ( 'NONE', *, *, #6270, .F. ) ;
#10006 = CARTESIAN_POINT ( 'NONE',  ( 82.99999999999998579, 8.660254037844390851, 205.0000000000000284 ) ) ;
#10007 = AXIS2_PLACEMENT_3D ( 'NONE', #9719, #13045, #5222 ) ;
#10008 = ADVANCED_FACE ( 'NONE', ( #8323 ), #10480, .T. ) ;
#10009 = PRODUCT_DEFINITION_SHAPE ( 'NONE', 'NONE',  #14314 ) ;
#10010 = EDGE_LOOP ( 'NONE', ( #7017, #13526, #11985, #9666 ) ) ;
#10011 = ORIENTED_EDGE ( 'NONE', *, *, #5095, .F. ) ;
#10012 = CARTESIAN_POINT ( 'NONE',  ( 0.000000000000000000, 1.438959988998140160E-15, -11.75000000000000000 ) ) ;
#10013 = LINE ( 'NONE', #8986, #14303 ) ;
#10014 = CARTESIAN_POINT ( 'NONE',  ( 209.9999999999999716, -85.00000000000007105, 169.9999999999999716 ) ) ;
#10015 = CARTESIAN_POINT ( 'NONE',  ( 1.800000000000002931, 0.000000000000000000, -13.50000000000000178 ) ) ;
#10016 = DIRECTION ( 'NONE',  ( -1.000000000000000000, -0.000000000000000000, -0.000000000000000000 ) ) ;
#10017 = DIRECTION ( 'NONE',  ( 0.000000000000000000, 0.000000000000000000, 1.000000000000000000 ) ) ;
#10018 = CIRCLE ( 'NONE', #7695, 5.560781378645573980 ) ;
#10019 = CARTESIAN_POINT ( 'NONE',  ( 197.5000000000000000, -90.00000000000007105, 55.00000000000001421 ) ) ;
#10020 = ADVANCED_FACE ( 'NONE', ( #3693 ), #12606, .T. ) ;
#10021 = FACE_OUTER_BOUND ( 'NONE', #7746, .T. ) ;
#10022 = AXIS2_PLACEMENT_3D ( 'NONE', #5067, #5139, #7368 ) ;
#10023 = ORIENTED_EDGE ( 'NONE', *, *, #3749, .T. ) ;
#10024 = PRESENTATION_LAYER_ASSIGNMENT (  '', '', ( #4003 ) ) ;
#10025 = ORIENTED_EDGE ( 'NONE', *, *, #900, .T. ) ;
#10026 = CARTESIAN_POINT ( 'NONE',  ( 2.740000000000000213, 0.5150000000000035660, -0.9838866223905657904 ) ) ;
#10027 =( REPRESENTATION_RELATIONSHIP ('NONE','NONE', #11251, #9307 ) REPRESENTATION_RELATIONSHIP_WITH_TRANSFORMATION ( #470 )SHAPE_REPRESENTATION_RELATIONSHIP( ) );
#10028 = ORIENTED_EDGE ( 'NONE', *, *, #5081, .T. ) ;
#10029 = FACE_OUTER_BOUND ( 'NONE', #7851, .T. ) ;
#10030 = AXIS2_PLACEMENT_3D ( 'NONE', #1, #2352, #948 ) ;
#10031 = ORIENTED_EDGE ( 'NONE', *, *, #6484, .F. ) ;
#10032 = DIRECTION ( 'NONE',  ( 0.000000000000000000, 0.000000000000000000, -1.000000000000000000 ) ) ;
#10033 = ORIENTED_EDGE ( 'NONE', *, *, #9037, .F. ) ;
#10034 = FACE_OUTER_BOUND ( 'NONE', #14061, .T. ) ;
#10035 = DIRECTION ( 'NONE',  ( 0.000000000000000000, -3.606821995490527259E-15, 1.000000000000000000 ) ) ;
#10036 = CARTESIAN_POINT ( 'NONE',  ( 4.211140560182196957, 2.431303136016536470, -3.745885042887433514 ) ) ;
#10037 = CARTESIAN_POINT ( 'NONE',  ( -30.00000000000002842, -20.00000000000000000, 240.0000000000000284 ) ) ;
#10038 = FACE_OUTER_BOUND ( 'NONE', #9705, .T. ) ;
#10039 = SURFACE_STYLE_USAGE ( .BOTH. , #1092 ) ;
#10040 = EDGE_CURVE ( 'NONE', #8357, #10068, #13024, .T. ) ;
#10041 = PLANE ( 'NONE',  #12676 ) ;
#10042 = AXIS2_PLACEMENT_3D ( 'NONE', #7251, #3918, #7172 ) ;
#10043 = VERTEX_POINT ( 'NONE', #390 ) ;
#10044 = EDGE_LOOP ( 'NONE', ( #10740, #10716, #3689, #7938 ) ) ;
#10045 = FACE_OUTER_BOUND ( 'NONE', #12941, .T. ) ;
#10046 = ORIENTED_EDGE ( 'NONE', *, *, #13299, .F. ) ;
#10047 = CARTESIAN_POINT ( 'NONE',  ( 136.6666666666666288, -20.00000000000000000, -222.5000000000000853 ) ) ;
#10048 = CYLINDRICAL_SURFACE ( 'NONE', #9669, 2.649999999999985700 ) ;
#10049 = EDGE_CURVE ( 'NONE', #11323, #3798, #7201, .T. ) ;
#10050 = EDGE_CURVE ( 'NONE', #2665, #10963, #13519, .T. ) ;
#10051 = CARTESIAN_POINT ( 'NONE',  ( 2.500000000000000000, 0.000000000000000000, 0.000000000000000000 ) ) ;
#10052 = EDGE_CURVE ( 'NONE', #12598, #12386, #5843, .T. ) ;
#10053 = CARTESIAN_POINT ( 'NONE',  ( 1.799999999999996048, 0.000000000000000000, -10.20000000000000107 ) ) ;
#10054 = DIRECTION ( 'NONE',  ( -1.000000000000000000, -0.000000000000000000, -0.000000000000000000 ) ) ;
#10055 = PRODUCT ( 'stationary aligner', 'stationary aligner', '', ( #10612 ) ) ;
#10056 = DIRECTION ( 'NONE',  ( -0.000000000000000000, -0.000000000000000000, 1.000000000000000000 ) ) ;
#10057 = ORIENTED_EDGE ( 'NONE', *, *, #5447, .T. ) ;
#10058 = DIRECTION ( 'NONE',  ( 0.000000000000000000, 0.000000000000000000, -1.000000000000000000 ) ) ;
#10059 = CARTESIAN_POINT ( 'NONE',  ( 2.500000000000000000, 1.768423874527822681, -1.021000000000002794 ) ) ;
#10060 = FACE_OUTER_BOUND ( 'NONE', #14057, .T. ) ;
#10061 = EDGE_LOOP ( 'NONE', ( #9792, #13645, #13082, #7835 ) ) ;
#10062 = DIRECTION ( 'NONE',  ( -1.000000000000000000, -0.000000000000000000, -0.000000000000000000 ) ) ;
#10063 = DIRECTION ( 'NONE',  ( -0.000000000000000000, -0.000000000000000000, 1.000000000000000000 ) ) ;
#10064 = DIRECTION ( 'NONE',  ( 6.123233995736766036E-17, -1.000000000000000000, 0.000000000000000000 ) ) ;
#10065 = ADVANCED_FACE ( 'NONE', ( #9254 ), #368, .T. ) ;
#10066 = ORIENTED_EDGE ( 'NONE', *, *, #3329, .F. ) ;
#10067 = CARTESIAN_POINT ( 'NONE',  ( 219.9999999999999716, -25.00000000000000000, -219.8500000000001080 ) ) ;
#10068 = VERTEX_POINT ( 'NONE', #9033 ) ;
#10069 = CARTESIAN_POINT ( 'NONE',  ( 0.000000000000000000, 0.000000000000000000, -186.0000000000000000 ) ) ;
#10070 = ORIENTED_EDGE ( 'NONE', *, *, #9969, .T. ) ;
#10071 = EDGE_LOOP ( 'NONE', ( #1639, #7594, #9394, #4016, #9952 ) ) ;
#10072 = CYLINDRICAL_SURFACE ( 'NONE', #6160, 5.500000000000005329 ) ;
#10073 = DIRECTION ( 'NONE',  ( -1.000000000000000000, -0.000000000000000000, -0.000000000000000000 ) ) ;
#10074 = APPLICATION_CONTEXT ( 'automotive_design' ) ;
#10075 = AXIS2_PLACEMENT_3D ( 'NONE', #9169, #13589, #5907 ) ;
#10076 = FACE_OUTER_BOUND ( 'NONE', #5951, .T. ) ;
#10077 = CARTESIAN_POINT ( 'NONE',  ( 303.3333333333333144, -20.00000000000000000, 219.8500000000001080 ) ) ;
#10078 = CARTESIAN_POINT ( 'NONE',  ( 0.000000000000000000, -1.178949249685213863, 2.042000000000002924 ) ) ;
#10079 = DIRECTION ( 'NONE',  ( -0.000000000000000000, 0.000000000000000000, 1.000000000000000000 ) ) ;
#10080 = DIRECTION ( 'NONE',  ( 0.000000000000000000, -0.000000000000000000, 1.000000000000000000 ) ) ;
#10081 = CONTEXT_DEPENDENT_SHAPE_REPRESENTATION ( #7240, #4972 ) ;
#10082 = ORIENTED_EDGE ( 'NONE', *, *, #11731, .F. ) ;
#10083 = EDGE_CURVE ( 'NONE', #12108, #12386, #5697, .T. ) ;
#10084 = ORIENTED_EDGE ( 'NONE', *, *, #8891, .F. ) ;
#10085 = CARTESIAN_POINT ( 'NONE',  ( 386.6666666666666288, -15.00000000000000000, 219.8500000000001080 ) ) ;
#10086 = AXIS2_PLACEMENT_3D ( 'NONE', #3838, #2754, #4206 ) ;
#10087 = VERTEX_POINT ( 'NONE', #11361 ) ;
#10088 = CARTESIAN_POINT ( 'NONE',  ( 25.00000000000000000, 0.000000000000000000, 0.000000000000000000 ) ) ;
#10089 = ORIENTED_EDGE ( 'NONE', *, *, #1129, .T. ) ;
#10090 = DIRECTION ( 'NONE',  ( 0.000000000000000000, 0.000000000000000000, 1.000000000000000000 ) ) ;
#10091 = VERTEX_POINT ( 'NONE', #11292 ) ;
#10092 = EDGE_CURVE ( 'NONE', #634, #2924, #10268, .T. ) ;
#10093 = FACE_OUTER_BOUND ( 'NONE', #2613, .T. ) ;
#10094 = FACE_OUTER_BOUND ( 'NONE', #6906, .T. ) ;
#10095 = DIRECTION ( 'NONE',  ( -1.000000000000000000, -0.000000000000000000, -0.000000000000000000 ) ) ;
#10096 = CARTESIAN_POINT ( 'NONE',  ( 53.33333333333330017, -14.99999999999999822, 222.5000000000000853 ) ) ;
#10097 = AXIS2_PLACEMENT_3D ( 'NONE', #13496, #3504, #4519 ) ;
#10098 = FACE_OUTER_BOUND ( 'NONE', #10724, .T. ) ;
#10099 =( NAMED_UNIT ( * ) SI_UNIT ( $, .STERADIAN. ) SOLID_ANGLE_UNIT ( ) );
#10100 = CARTESIAN_POINT ( 'NONE',  ( 137.4999999999999432, -56.99999999999997158, -169.9999999999999716 ) ) ;
#10101 = ORIENTED_EDGE ( 'NONE', *, *, #7615, .T. ) ;
#10102 = VERTEX_POINT ( 'NONE', #13452 ) ;
#10103 = VERTEX_POINT ( 'NONE', #10059 ) ;
#10104 = DIRECTION ( 'NONE',  ( 0.000000000000000000, -1.000000000000000000, 0.000000000000000000 ) ) ;
#10105 = ORIENTED_EDGE ( 'NONE', *, *, #14017, .F. ) ;
#10106 = CARTESIAN_POINT ( 'NONE',  ( 219.9999999999999716, -85.00000000000007105, 55.00000000000002132 ) ) ;
#10107 = ADVANCED_FACE ( 'NONE', ( #5770 ), #6075, .F. ) ;
#10108 = CARTESIAN_POINT ( 'NONE',  ( -30.00000000000002842, -25.00000000000000000, 250.0000000000000000 ) ) ;
#10109 = AXIS2_PLACEMENT_3D ( 'NONE', #10856, #5058, #11792 ) ;
#10110 = EDGE_CURVE ( 'NONE', #13622, #1918, #230, .T. ) ;
#10111 = CARTESIAN_POINT ( 'NONE',  ( 211.3397459621556038, -80.00000000000007105, 50.00000000000001421 ) ) ;
#10112 = AXIS2_PLACEMENT_3D ( 'NONE', #1631, #1414, #11439 ) ;
#10113 = CARTESIAN_POINT ( 'NONE',  ( 0.000000000000000000, 0.000000000000000000, 0.000000000000000000 ) ) ;
#10114 = CARTESIAN_POINT ( 'NONE',  ( 470.0000000000000000, -25.00000000000000000, -169.9999999999999716 ) ) ;
#10115 = AXIS2_PLACEMENT_3D ( 'NONE', #11655, #10418, #12452 ) ;
#10116 = VECTOR ( 'NONE', #1937, 1000.000000000000114 ) ;
#10117 = FACE_OUTER_BOUND ( 'NONE', #14090, .T. ) ;
#10118 = DIRECTION ( 'NONE',  ( 0.000000000000000000, 0.000000000000000000, 1.000000000000000000 ) ) ;
#10119 = EDGE_CURVE ( 'NONE', #10068, #1770, #8621, .T. ) ;
#10120 = AXIS2_PLACEMENT_3D ( 'NONE', #2626, #1082, #6757 ) ;
#10121 = EDGE_LOOP ( 'NONE', ( #9580, #13145, #6898, #5970, #12932 ) ) ;
#10122 = CIRCLE ( 'NONE', #1311, 2.041999999999999815 ) ;
#10123 = CARTESIAN_POINT ( 'NONE',  ( 0.000000000000000000, 0.000000000000000000, 200.0000000000000000 ) ) ;
#10124 = EDGE_CURVE ( 'NONE', #4728, #5839, #3740, .T. ) ;
#10125 = CARTESIAN_POINT ( 'NONE',  ( 5.200000000000002842, 0.000000000000000000, 0.000000000000000000 ) ) ;
#10126 = FACE_OUTER_BOUND ( 'NONE', #1423, .T. ) ;
#10127 = ORIENTED_EDGE ( 'NONE', *, *, #7997, .T. ) ;
#10128 = AXIS2_PLACEMENT_3D ( 'NONE', #3781, #13553, #9142 ) ;
#10129 = CIRCLE ( 'NONE', #13826, 2.649999999999985700 ) ;
#10130 = LINE ( 'NONE', #5495, #12656 ) ;
#10131 = CARTESIAN_POINT ( 'NONE',  ( 2.500000000000000888, 3.061616997868384127E-16, -4.974599999999998801 ) ) ;
#10132 = DIRECTION ( 'NONE',  ( 0.000000000000000000, 0.000000000000000000, 1.000000000000000000 ) ) ;
#10133 = AXIS2_PLACEMENT_3D ( 'NONE', #12846, #6176, #3857 ) ;
#10134 = CONTEXT_DEPENDENT_SHAPE_REPRESENTATION ( #5029, #4284 ) ;
#10135 = EDGE_CURVE ( 'NONE', #2919, #3667, #88, .T. ) ;
#10136 =( GEOMETRIC_REPRESENTATION_CONTEXT ( 3 ) GLOBAL_UNCERTAINTY_ASSIGNED_CONTEXT ( ( #11855 ) ) GLOBAL_UNIT_ASSIGNED_CONTEXT ( ( #852, #11032, #13124 ) ) REPRESENTATION_CONTEXT ( 'NONE', 'WORKASPACE' ) );
#10137 = EDGE_CURVE ( 'NONE', #1103, #10087, #2610, .T. ) ;
#10138 = EDGE_LOOP ( 'NONE', ( #11984, #13055, #2891, #3878 ) ) ;
#10139 = PRESENTATION_LAYER_ASSIGNMENT (  '', '', ( #13607 ) ) ;
#10140 = CARTESIAN_POINT ( 'NONE',  ( 305.4999999999999432, -75.00000000000008527, 190.0000000000000000 ) ) ;
#10141 = ORIENTED_EDGE ( 'NONE', *, *, #6939, .F. ) ;
#10142 = CARTESIAN_POINT ( 'NONE',  ( 2.725741868436127202, -3.045094352033990148, -3.220599429844051453 ) ) ;
#10143 = EDGE_CURVE ( 'NONE', #6597, #4143, #14174, .T. ) ;
#10144 = ORIENTED_EDGE ( 'NONE', *, *, #9285, .T. ) ;
#10145 = VERTEX_POINT ( 'NONE', #12307 ) ;
#10146 = CARTESIAN_POINT ( 'NONE',  ( 236.4999999999999432, -85.00000000000007105, 190.0000000000000000 ) ) ;
#10147 = DIRECTION ( 'NONE',  ( 0.000000000000000000, 1.000000000000000000, -1.471414886128461471E-15 ) ) ;
#10148 = CARTESIAN_POINT ( 'NONE',  ( 0.000000000000000000, 0.000000000000000000, 190.0000000000000000 ) ) ;
#10149=STYLED_ITEM('',(#14424),#13412);
#10150 = DIRECTION ( 'NONE',  ( -0.000000000000000000, 1.000000000000000000, -0.000000000000000000 ) ) ;
#10151 = CARTESIAN_POINT ( 'NONE',  ( 140.0000000000000000, -95.00000000000008527, 190.0000000000000000 ) ) ;
#10152 = DIRECTION ( 'NONE',  ( 0.000000000000000000, 0.000000000000000000, -1.000000000000000000 ) ) ;
#10153 = DIRECTION ( 'NONE',  ( -1.000000000000000000, 0.000000000000000000, 0.000000000000000000 ) ) ;
#10154 = ORIENTED_EDGE ( 'NONE', *, *, #10368, .T. ) ;
#10155 = ORIENTED_EDGE ( 'NONE', *, *, #14276, .T. ) ;
#10156 = DIRECTION ( 'NONE',  ( 1.000000000000000000, 0.000000000000000000, 0.000000000000000000 ) ) ;
#10157 = EDGE_LOOP ( 'NONE', ( #5086, #3350, #3155, #13100 ) ) ;
#10158 = CARTESIAN_POINT ( 'NONE',  ( -135.0000000000000000, -75.00000000000008527, -14.14213562373090127 ) ) ;
#10159 = CIRCLE ( 'NONE', #1823, 4.250000000000000000 ) ;
#10160 = ORIENTED_EDGE ( 'NONE', *, *, #3806, .F. ) ;
#10161 = CARTESIAN_POINT ( 'NONE',  ( -31.74999999999995737, 5.204748896376250699E-16, -4.250000000000000000 ) ) ;
#10162 = EDGE_LOOP ( 'NONE', ( #17, #11377, #3180, #3682 ) ) ;
#10163 = CONICAL_SURFACE ( 'NONE', #11328, 2.500000000000002220, 1.029744260000002631 ) ;
#10164 = LINE ( 'NONE', #124, #4766 ) ;
#10165 = PRODUCT ( 'pan head cross recess screw_iso_ISO 7045 - M5 x 25 - Z - 25N', 'pan head cross recess screw_iso_ISO 7045 - M5 x 25 - Z - 25N', '', ( #5961 ) ) ;
#10166 = DIRECTION ( 'NONE',  ( 0.000000000000000000, -0.5000000000000012212, -0.8660254037844380415 ) ) ;
#10167 = PRESENTATION_STYLE_ASSIGNMENT (( #5741 ) ) ;
#10168 = ADVANCED_FACE ( 'NONE', ( #7864 ), #9174, .T. ) ;
#10169 = CYLINDRICAL_SURFACE ( 'NONE', #12496, 2.649999999999985700 ) ;
#10170 = AXIS2_PLACEMENT_3D ( 'NONE', #13334, #9870, #10968 ) ;
#10171 = SURFACE_STYLE_FILL_AREA ( #11059 ) ;
#10172 = DIRECTION ( 'NONE',  ( 1.000000000000000000, 0.000000000000000000, 6.123233995736766036E-17 ) ) ;
#10173 = FACE_BOUND ( 'NONE', #13994, .T. ) ;
#10174 = ORIENTED_EDGE ( 'NONE', *, *, #872, .F. ) ;
#10175 = CONICAL_SURFACE ( 'NONE', #7855, 2.041999999999999815, 1.047197551196591858 ) ;
#10176 = VERTEX_POINT ( 'NONE', #8083 ) ;
#10177 = VERTEX_POINT ( 'NONE', #2584 ) ;
#10178 = CARTESIAN_POINT ( 'NONE',  ( 4.000000000000000000, -2.309401076758514915, -3.433295621305383349 ) ) ;
#10179 = EDGE_LOOP ( 'NONE', ( #14114, #2265 ) ) ;
#10180 = CARTESIAN_POINT ( 'NONE',  ( -31.74999999999995737, 0.000000000000000000, 0.000000000000000000 ) ) ;
#10181 = DIRECTION ( 'NONE',  ( 0.000000000000000000, 0.000000000000000000, 1.000000000000000000 ) ) ;
#10182 = ADVANCED_FACE ( 'NONE', ( #7004 ), #158, .F. ) ;
#10183 = PLANE ( 'NONE',  #12695 ) ;
#10184 = AXIS2_PLACEMENT_3D ( 'NONE', #2646, #11428, #360 ) ;
#10185 = LINE ( 'NONE', #1394, #5380 ) ;
#10186 = AXIS2_PLACEMENT_3D ( 'NONE', #6213, #8454, #5141 ) ;
#10187 = AXIS2_PLACEMENT_3D ( 'NONE', #9590, #5174, #8414 ) ;
#10188 = DIRECTION ( 'NONE',  ( -0.000000000000000000, -0.000000000000000000, 1.000000000000000000 ) ) ;
#10189 = DIRECTION ( 'NONE',  ( -1.000000000000000000, -0.000000000000000000, -0.000000000000000000 ) ) ;
#10190 = FACE_OUTER_BOUND ( 'NONE', #7565, .T. ) ;
#10191 = EDGE_CURVE ( 'NONE', #4081, #930, #6795, .T. ) ;
#10192 = VERTEX_POINT ( 'NONE', #3887 ) ;
#10193 = ADVANCED_FACE ( 'NONE', ( #9398 ), #3960, .T. ) ;
#10194 =( NAMED_UNIT ( * ) PLANE_ANGLE_UNIT ( ) SI_UNIT ( $, .RADIAN. ) );
#10195 = VECTOR ( 'NONE', #499, 1000.000000000000000 ) ;
#10196 = CARTESIAN_POINT ( 'NONE',  ( 219.9999999999999716, -20.00000000000000000, 219.8500000000001080 ) ) ;
#10197 = CARTESIAN_POINT ( 'NONE',  ( -145.0000000000000284, -95.00000000000008527, -14.14213562373090127 ) ) ;
#10198 = EDGE_LOOP ( 'NONE', ( #8117, #12714 ) ) ;
#10199 = AXIS2_PLACEMENT_3D ( 'NONE', #2428, #11278, #12298 ) ;
#10200 = DIRECTION ( 'NONE',  ( -1.000000000000000000, 0.000000000000000000, -0.000000000000000000 ) ) ;
#10201 = LINE ( 'NONE', #10131, #10877 ) ;
#10202 = DIRECTION ( 'NONE',  ( 1.000000000000000000, 0.000000000000000000, 0.000000000000000000 ) ) ;
#10203 = VECTOR ( 'NONE', #13113, 1000.000000000000000 ) ;
#10204 =( REPRESENTATION_RELATIONSHIP ('NONE','NONE', #11251, #7730 ) REPRESENTATION_RELATIONSHIP_WITH_TRANSFORMATION ( #10805 )SHAPE_REPRESENTATION_RELATIONSHIP( ) );
#10205 = ADVANCED_FACE ( 'NONE', ( #7145 ), #13708, .T. ) ;
#10206 = EDGE_CURVE ( 'NONE', #9383, #7171, #10561, .T. ) ;
#10207=STYLED_ITEM('',(#14417),#3687);
#10208 = ORIENTED_EDGE ( 'NONE', *, *, #5278, .T. ) ;
#10209 = DIRECTION ( 'NONE',  ( 1.000000000000000000, 0.000000000000000000, 0.000000000000000000 ) ) ;
#10210 = EDGE_LOOP ( 'NONE', ( #5015, #8859 ) ) ;
#10211 = CARTESIAN_POINT ( 'NONE',  ( 1.360585162435110629, -4.061296242128317857, -3.505054077164905024 ) ) ;
#10212 = CIRCLE ( 'NONE', #3285, 2.649999999999985700 ) ;
#10213 = ORIENTED_EDGE ( 'NONE', *, *, #11550, .F. ) ;
#10214 = ORIENTED_EDGE ( 'NONE', *, *, #2246, .F. ) ;
#10215 = CARTESIAN_POINT ( 'NONE',  ( 82.99999999999998579, -8.660254037844389075, 199.9990000000000236 ) ) ;
#10216 = EDGE_CURVE ( 'NONE', #6474, #8679, #1903, .T. ) ;
#10217 = ADVANCED_FACE ( 'NONE', ( #1847 ), #1767, .F. ) ;
#10218 = FACE_OUTER_BOUND ( 'NONE', #8949, .T. ) ;
#10219 = DIRECTION ( 'NONE',  ( 1.000000000000000000, 0.000000000000000000, 0.000000000000000000 ) ) ;
#10220 = EDGE_CURVE ( 'NONE', #1514, #7747, #10951, .T. ) ;
#10221 = CIRCLE ( 'NONE', #3969, 2.500000000000002220 ) ;
#10222 = CARTESIAN_POINT ( 'NONE',  ( 0.000000000000000000, 0.000000000000000000, -5.000000000000000000 ) ) ;
#10223 = DIRECTION ( 'NONE',  ( -0.8571673013836870192, 1.049727191973306873E-16, 0.5150380737757234151 ) ) ;
#10224 = CARTESIAN_POINT ( 'NONE',  ( 434.9999999999999432, 8.660254037844390851, 200.0000000000000000 ) ) ;
#10225 = CARTESIAN_POINT ( 'NONE',  ( 4.211140560182196957, -2.431303136016555122, -3.745885042887436622 ) ) ;
#10226 = CONTEXT_DEPENDENT_SHAPE_REPRESENTATION ( #260, #5440 ) ;
#10227 = CIRCLE ( 'NONE', #7445, 0.8509999999999999787 ) ;
#10228 = EDGE_LOOP ( 'NONE', ( #987, #13966, #4599, #7411 ) ) ;
#10229 = ORIENTED_EDGE ( 'NONE', *, *, #3329, .T. ) ;
#10230 = DIRECTION ( 'NONE',  ( -0.000000000000000000, 1.000000000000000000, -0.000000000000000000 ) ) ;
#10231 = EDGE_LOOP ( 'NONE', ( #7949, #2112, #13821, #3019 ) ) ;
#10232 = DIRECTION ( 'NONE',  ( -1.000000000000000000, 0.000000000000000000, 0.000000000000000000 ) ) ;
#10233 = ORIENTED_EDGE ( 'NONE', *, *, #4522, .F. ) ;
#10234 = DIRECTION ( 'NONE',  ( -0.000000000000000000, -1.000000000000000000, -0.000000000000000000 ) ) ;
#10235 = ORIENTED_EDGE ( 'NONE', *, *, #10293, .F. ) ;
#10236 = CARTESIAN_POINT ( 'NONE',  ( 294.4999999999999432, -95.00000000000008527, 186.2999999999999829 ) ) ;
#10237 = DIRECTION ( 'NONE',  ( -1.000000000000000000, 0.000000000000000000, 0.000000000000000000 ) ) ;
#10239 = ORIENTED_EDGE ( 'NONE', *, *, #7159, .F. ) ;
#10238 = VECTOR ( 'NONE', #6881, 1000.000000000000000 ) ;
#10240 = LINE ( 'NONE', #410, #4847 ) ;
#10241 = AXIS2_PLACEMENT_3D ( 'NONE', #1901, #4154, #7693 ) ;
#10242 = SURFACE_SIDE_STYLE ('',( #275 ) ) ;
#10243 = DIRECTION ( 'NONE',  ( 0.000000000000000000, 0.000000000000000000, 1.000000000000000000 ) ) ;
#10244 = FACE_OUTER_BOUND ( 'NONE', #80, .T. ) ;
#10245 = ORIENTED_EDGE ( 'NONE', *, *, #8259, .F. ) ;
#10246 = ORIENTED_EDGE ( 'NONE', *, *, #5525, .F. ) ;
#10247 = AXIS2_PLACEMENT_3D ( 'NONE', #518, #6274, #9619 ) ;
#10248 = ORIENTED_EDGE ( 'NONE', *, *, #11946, .T. ) ;
#10249 = ADVANCED_FACE ( 'NONE', ( #7217 ), #12810, .F. ) ;
#10250 = CARTESIAN_POINT ( 'NONE',  ( 303.3333333333333144, -20.00000000000000000, -222.5000000000000853 ) ) ;
#10251 = PRODUCT_DEFINITION_FORMATION_WITH_SPECIFIED_SOURCE ( 'ANY', '', #59, .NOT_KNOWN. ) ;
#10252 = B_SPLINE_CURVE_WITH_KNOTS ( 'NONE', 3,
 ( #3284, #5383, #1071, #3360, #13131, #12997 ),
 .UNSPECIFIED., .F., .F.,
 ( 4, 2, 4 ),
 ( 0.002365888236227977302, 0.003551327329835078910, 0.004736766423442180518 ),
 .UNSPECIFIED. ) ;
#10253 = COLOUR_RGB ( '',0.8941176470588234615, 0.8941176470588234615, 0.8941176470588234615 ) ;
#10254 = ORIENTED_EDGE ( 'NONE', *, *, #8718, .T. ) ;
#10255 = DIRECTION ( 'NONE',  ( -0.000000000000000000, -0.000000000000000000, 1.000000000000000000 ) ) ;
#10256 = ORIENTED_EDGE ( 'NONE', *, *, #2241, .F. ) ;
#10257 = LINE ( 'NONE', #285, #3417 ) ;
#10258 = DIRECTION ( 'NONE',  ( 0.000000000000000000, 0.4999999999999990008, -0.8660254037844391517 ) ) ;
#10259 = VECTOR ( 'NONE', #8523, 1000.000000000000000 ) ;
#10260 = DIRECTION ( 'NONE',  ( -0.000000000000000000, 1.000000000000000000, -0.000000000000000000 ) ) ;
#10261 = FACE_OUTER_BOUND ( 'NONE', #6305, .T. ) ;
#10262 = CARTESIAN_POINT ( 'NONE',  ( 145.5000000000000284, -75.00000000000008527, -190.0000000000000000 ) ) ;
#10263 = CARTESIAN_POINT ( 'NONE',  ( 219.9999999999999716, -20.00000000000000000, 222.5000000000000853 ) ) ;
#10264 = CARTESIAN_POINT ( 'NONE',  ( -1.799999999999996048, 0.000000000000000000, 0.000000000000000000 ) ) ;
#10265 = ORIENTED_EDGE ( 'NONE', *, *, #13840, .T. ) ;
#10266 = APPLICATION_CONTEXT ( 'automotive_design' ) ;
#10267 = CARTESIAN_POINT ( 'NONE',  ( 8.000000000000000000, 0.5150000000000000133, 1.798112889504231112E-15 ) ) ;
#10268 = LINE ( 'NONE', #4619, #8866 ) ;
#10269 = PRESENTATION_STYLE_ASSIGNMENT (( #7006 ) ) ;
#10270 = ORIENTED_EDGE ( 'NONE', *, *, #2065, .F. ) ;
#10271 = EDGE_CURVE ( 'NONE', #8555, #5301, #12651, .T. ) ;
#10272 = CARTESIAN_POINT ( 'NONE',  ( 305.4999999999999432, -95.00000000000008527, 190.0000000000000000 ) ) ;
#10273 = DIRECTION ( 'NONE',  ( 0.000000000000000000, -0.4999999999999993339, 0.8660254037844390407 ) ) ;
#10274 = CARTESIAN_POINT ( 'NONE',  ( 176.0000000000000000, 0.000000000000000000, 0.000000000000000000 ) ) ;
#10275 = DIRECTION ( 'NONE',  ( 0.000000000000000000, 0.000000000000000000, 1.000000000000000000 ) ) ;
#10276 = ORIENTED_EDGE ( 'NONE', *, *, #7745, .T. ) ;
#10277 = CARTESIAN_POINT ( 'NONE',  ( 4.999999999999997335, 0.000000000000000000, 0.000000000000000000 ) ) ;
#10278 = PRODUCT_DEFINITION_SHAPE ( 'NONE', 'NONE',  #14311 ) ;
#10279 = ORIENTED_EDGE ( 'NONE', *, *, #3043, .T. ) ;
#10280 = DIRECTION ( 'NONE',  ( 0.000000000000000000, 0.000000000000000000, -1.000000000000000000 ) ) ;
#10281 = EDGE_LOOP ( 'NONE', ( #9457, #12152, #12402, #4672 ) ) ;
#10282 = VERTEX_POINT ( 'NONE', #7361 ) ;
#10284 = ADVANCED_FACE ( 'NONE', ( #10712 ), #741, .F. ) ;
#10283 = FACE_OUTER_BOUND ( 'NONE', #6798, .T. ) ;
#10285 = CARTESIAN_POINT ( 'NONE',  ( -0.1410422978106123659, 4.700232962125094893, -3.687027686973624707 ) ) ;
#10286 = DIRECTION ( 'NONE',  ( -0.5000000000000051070, 1.060575238724903217E-16, -0.8660254037844355990 ) ) ;
#10287 = DIRECTION ( 'NONE',  ( -1.000000000000000000, 0.000000000000000000, 0.000000000000000000 ) ) ;
#10288 = CARTESIAN_POINT ( 'NONE',  ( -294.9999999999999432, -95.00000000000008527, 354.1421356237308942 ) ) ;
#10289 =( NAMED_UNIT ( * ) PLANE_ANGLE_UNIT ( ) SI_UNIT ( $, .RADIAN. ) );
#10290 = CARTESIAN_POINT ( 'NONE',  ( 2.344047193898588954, 3.265465875126468021, -5.031375706690542042E-16 ) ) ;
#10291 = EDGE_LOOP ( 'NONE', ( #3629, #4893, #11994, #12614 ) ) ;
#10292 = ORIENTED_EDGE ( 'NONE', *, *, #13568, .F. ) ;
#10293 = EDGE_CURVE ( 'NONE', #13284, #13567, #4034, .T. ) ;
#10294 = EDGE_CURVE ( 'NONE', #2887, #1982, #12588, .T. ) ;
#10295 = CARTESIAN_POINT ( 'NONE',  ( 24.55500000000002103, 0.000000000000000000, 0.000000000000000000 ) ) ;
#10296 = VERTEX_POINT ( 'NONE', #670 ) ;
#10297 = CARTESIAN_POINT ( 'NONE',  ( -30.00000000000002842, -20.00000000000000000, 250.0000000000000000 ) ) ;
#10298 = ORIENTED_EDGE ( 'NONE', *, *, #6938, .T. ) ;
#10299 = PLANE ( 'NONE',  #10128 ) ;
#10300 = VERTEX_POINT ( 'NONE', #2651 ) ;
#10302 = EDGE_CURVE ( 'NONE', #546, #12712, #6548, .T. ) ;
#10301 = CARTESIAN_POINT ( 'NONE',  ( 0.2277608394786177770, 0.000000000000000000, 10.72500000000000142 ) ) ;
#10303 = LINE ( 'NONE', #3709, #144 ) ;
#10304 = VERTEX_POINT ( 'NONE', #9472 ) ;
#10305 = DIRECTION ( 'NONE',  ( -0.000000000000000000, 1.000000000000000000, -0.000000000000000000 ) ) ;
#10306 = CARTESIAN_POINT ( 'NONE',  ( 4.211140560182196957, 2.431303136016536470, -3.745885042887433514 ) ) ;
#10307 = FILL_AREA_STYLE_COLOUR ( '', #436 ) ;
#10308 = SHAPE_DEFINITION_REPRESENTATION ( #11097, #4229 ) ;
#10309 = CARTESIAN_POINT ( 'NONE',  ( 2.000000000000001776, 1.524685264938454646E-15, 12.44999999999999929 ) ) ;
#10310 = AXIS2_PLACEMENT_3D ( 'NONE', #10517, #13698, #8471 ) ;
#10311 = EDGE_LOOP ( 'NONE', ( #6547, #3157 ) ) ;
#10312 = ADVANCED_FACE ( 'NONE', ( #8443 ), #1623, .T. ) ;
#10313 = ORIENTED_EDGE ( 'NONE', *, *, #3235, .F. ) ;
#10314 = SHAPE_REPRESENTATION ( 'socket head cap screw_iso_ISO 4762 M5 x 16 - 16N', ( #14039 ), #1895 ) ;
#10315 = VERTEX_POINT ( 'NONE', #8376 ) ;
#10316 = CARTESIAN_POINT ( 'NONE',  ( 302.4999999999999432, 45.00000000000001421, 0.000000000000000000 ) ) ;
#10317 = ORIENTED_EDGE ( 'NONE', *, *, #10554, .F. ) ;
#10318 = DIRECTION ( 'NONE',  ( -1.000000000000000000, -0.000000000000000000, -0.000000000000000000 ) ) ;
#10319 = EDGE_LOOP ( 'NONE', ( #10980, #8881 ) ) ;
#10320 = FACE_OUTER_BOUND ( 'NONE', #14289, .T. ) ;
#10321 = EDGE_CURVE ( 'NONE', #10991, #8744, #10018, .T. ) ;
#10322 = AXIS2_PLACEMENT_3D ( 'NONE', #7630, #3296, #10909 ) ;
#10323 = DIRECTION ( 'NONE',  ( 0.000000000000000000, 0.000000000000000000, 1.000000000000000000 ) ) ;
#10324 = FACE_OUTER_BOUND ( 'NONE', #4733, .T. ) ;
#10325 = EDGE_CURVE ( 'NONE', #7171, #574, #3757, .T. ) ;
#10326 = CARTESIAN_POINT ( 'NONE',  ( -30.00000000000002842, -25.00000000000000000, -250.0000000000000000 ) ) ;
#10327 = CARTESIAN_POINT ( 'NONE',  ( 357.0000000000000000, 8.660254037844390851, 200.0000000000000000 ) ) ;
#10328 = CARTESIAN_POINT ( 'NONE',  ( 1.424271237134740131, 0.000000000000000000, 0.000000000000000000 ) ) ;
#10329 = CARTESIAN_POINT ( 'NONE',  ( 132.4999999999999432, -36.99999999999997868, -180.0000000000000000 ) ) ;
#10330 = ORIENTED_EDGE ( 'NONE', *, *, #13299, .T. ) ;
#10331 = AXIS2_PLACEMENT_3D ( 'NONE', #4567, #8918, #13196 ) ;
#10332 = CIRCLE ( 'NONE', #8751, 9.999999999999980460 ) ;
#10333 = LINE ( 'NONE', #13671, #4427 ) ;
#10334 = CARTESIAN_POINT ( 'NONE',  ( -31.74999999999995737, 0.000000000000000000, 0.000000000000000000 ) ) ;
#10335 = CARTESIAN_POINT ( 'NONE',  ( 229.9999999999999432, -85.00000000000007105, 55.00000000000002132 ) ) ;
#10336 = AXIS2_PLACEMENT_3D ( 'NONE', #7825, #12120, #12260 ) ;
#10337 = ORIENTED_EDGE ( 'NONE', *, *, #13959, .F. ) ;
#10338 = COLOUR_RGB ( '',1.000000000000000000, 0.9490196078431372140, 0.9098039215686274384 ) ;
#10339 = B_SPLINE_CURVE_WITH_KNOTS ( 'NONE', 3,
 ( #2307, #12171, #5855, #13527, #6732 ),
 .UNSPECIFIED., .F., .F.,
 ( 4, 1, 4 ),
 ( 0.000000000000000000, 0.002309401076758505356, 0.004618802153517010713 ),
 .UNSPECIFIED. ) ;
#10340 = AXIS2_PLACEMENT_3D ( 'NONE', #9607, #14013, #5120 ) ;
#10341 = LINE ( 'NONE', #8159, #11154 ) ;
#10342 = EDGE_CURVE ( 'NONE', #9188, #8841, #937, .T. ) ;
#10343 = AXIS2_PLACEMENT_3D ( 'NONE', #9832, #8137, #11556 ) ;
#10344 = CARTESIAN_POINT ( 'NONE',  ( 444.9999999999999432, 8.660254037844390851, 205.0000000000000284 ) ) ;
#10345 = DIRECTION ( 'NONE',  ( 1.000000000000000000, 0.000000000000000000, 0.000000000000000000 ) ) ;
#10346 = DIRECTION ( 'NONE',  ( 0.000000000000000000, 0.000000000000000000, 1.000000000000000000 ) ) ;
#10347 = CIRCLE ( 'NONE', #8962, 2.649999999999985700 ) ;
#10348 =( REPRESENTATION_RELATIONSHIP ('NONE','NONE', #11251, #9307 ) REPRESENTATION_RELATIONSHIP_WITH_TRANSFORMATION ( #7616 )SHAPE_REPRESENTATION_RELATIONSHIP( ) );
#10349 = ORIENTED_EDGE ( 'NONE', *, *, #8435, .F. ) ;
#10350 = DIRECTION ( 'NONE',  ( 0.000000000000000000, 0.000000000000000000, -1.000000000000000000 ) ) ;
#10351 = CARTESIAN_POINT ( 'NONE',  ( 1.999999999999997335, 10.20000000000000107, 0.000000000000000000 ) ) ;
#10352 = AXIS2_PLACEMENT_3D ( 'NONE', #3226, #8796, #13073 ) ;
#10353 = ORIENTED_EDGE ( 'NONE', *, *, #11185, .F. ) ;
#10354 = DIRECTION ( 'NONE',  ( 1.000000000000000000, 0.000000000000000000, 0.000000000000000000 ) ) ;
#10355 = CARTESIAN_POINT ( 'NONE',  ( 2.836893136758676270, 3.208949435745843903, -3.505054077164911241 ) ) ;
#10356 = VECTOR ( 'NONE', #9086, 1000.000000000000000 ) ;
#10357 = FACE_OUTER_BOUND ( 'NONE', #14244, .T. ) ;
#10358 = DIRECTION ( 'NONE',  ( 0.000000000000000000, -1.224646799147352468E-16, 1.000000000000000000 ) ) ;
#10359 = AXIS2_PLACEMENT_3D ( 'NONE', #4362, #2102, #12917 ) ;
#10360 = CARTESIAN_POINT ( 'NONE',  ( 0.000000000000000000, 0.000000000000000000, 0.000000000000000000 ) ) ;
#10361 = CARTESIAN_POINT ( 'NONE',  ( 2.500000000000000000, 0.000000000000000000, 0.000000000000000000 ) ) ;
#10362 = SURFACE_SIDE_STYLE ('',( #5936 ) ) ;
#10363 = CYLINDRICAL_SURFACE ( 'NONE', #14105, 20.00000000000000000 ) ;
#10364 = AXIS2_PLACEMENT_3D ( 'NONE', #3336, #3599, #11222 ) ;
#10365 = CIRCLE ( 'NONE', #9914, 2.500000000000002220 ) ;
#10366 = VERTEX_POINT ( 'NONE', #12730 ) ;
#10367 = ORIENTED_EDGE ( 'NONE', *, *, #1882, .T. ) ;
#10368 = EDGE_CURVE ( 'NONE', #8791, #2471, #4953, .T. ) ;
#10369 = DIRECTION ( 'NONE',  ( 1.000000000000000000, 0.000000000000000000, 0.000000000000000000 ) ) ;
#10370 = EDGE_CURVE ( 'NONE', #9196, #14235, #6424, .T. ) ;
#10371 = ORIENTED_EDGE ( 'NONE', *, *, #3065, .F. ) ;
#10372 = DIRECTION ( 'NONE',  ( 0.000000000000000000, 0.000000000000000000, 1.000000000000000000 ) ) ;
#10373 = PRESENTATION_LAYER_ASSIGNMENT (  '', '', ( #2232 ) ) ;
#10374 = EDGE_LOOP ( 'NONE', ( #8477, #10441 ) ) ;
#10375 = CARTESIAN_POINT ( 'NONE',  ( 119.9999999999999147, -225.0010000000000048, -169.9999999999999716 ) ) ;
#10376 = ORIENTED_EDGE ( 'NONE', *, *, #5865, .T. ) ;
#10377 = CARTESIAN_POINT ( 'NONE',  ( 0.000000000000000000, -1.178949249685214307, 2.042000000000001592 ) ) ;
#10378 = CARTESIAN_POINT ( 'NONE',  ( 299.9999999999999432, -75.00000000000008527, 186.2999999999999829 ) ) ;
#10379 = VERTEX_POINT ( 'NONE', #13086 ) ;
#10380 = DIRECTION ( 'NONE',  ( -0.000000000000000000, -0.000000000000000000, -1.000000000000000000 ) ) ;
#10381 = EDGE_CURVE ( 'NONE', #2540, #13072, #10996, .T. ) ;
#10382 = DIRECTION ( 'NONE',  ( -0.000000000000000000, -0.000000000000000000, -1.000000000000000000 ) ) ;
#10383 = DIRECTION ( 'NONE',  ( 1.000000000000000000, 0.000000000000000000, 0.000000000000000000 ) ) ;
#10384 = APPLICATION_PROTOCOL_DEFINITION ( 'draft international standard', 'automotive_design', 1998, #6572 ) ;
#10385 = PLANE ( 'NONE',  #6436 ) ;
#10386 = ORIENTED_EDGE ( 'NONE', *, *, #9968, .T. ) ;
#10387 = ADVANCED_FACE ( 'NONE', ( #2206, #6633 ), #1025, .F. ) ;
#10388 = ORIENTED_EDGE ( 'NONE', *, *, #9992, .T. ) ;
#10389 = EDGE_CURVE ( 'NONE', #9987, #6099, #7476, .T. ) ;
#10390 = ORIENTED_EDGE ( 'NONE', *, *, #11546, .T. ) ;
#10391 = DIRECTION ( 'NONE',  ( -0.000000000000000000, -0.000000000000000000, 1.000000000000000000 ) ) ;
#10392 = ADVANCED_FACE ( 'NONE', ( #9766 ), #10492, .F. ) ;
#10393 = VERTEX_POINT ( 'NONE', #5548 ) ;
#10394 = LINE ( 'NONE', #7056, #2465 ) ;
#10395 = VERTEX_POINT ( 'NONE', #13022 ) ;
#10396 = CARTESIAN_POINT ( 'NONE',  ( 79.99999999999971578, 55.00000000000000711, 10.00000000000000000 ) ) ;
#10397 = FACE_OUTER_BOUND ( 'NONE', #14266, .T. ) ;
#10398 = CARTESIAN_POINT ( 'NONE',  ( 4.211140560182196957, 2.431303136016536470, -3.745885042887433514 ) ) ;
#10399 = CIRCLE ( 'NONE', #5996, 2.649999999999985700 ) ;
#10400 = EDGE_CURVE ( 'NONE', #13361, #8184, #264, .T. ) ;
#10401 = EDGE_CURVE ( 'NONE', #278, #2622, #7575, .T. ) ;
#10402 = DIRECTION ( 'NONE',  ( 0.000000000000000000, -0.000000000000000000, -1.000000000000000000 ) ) ;
#10403 = EDGE_CURVE ( 'NONE', #12400, #7986, #12082, .T. ) ;
#10404 = DIRECTION ( 'NONE',  ( -1.000000000000000000, 0.000000000000000000, 0.000000000000000000 ) ) ;
#10405 = CIRCLE ( 'NONE', #4393, 5.500000000000005329 ) ;
#10406 = DIRECTION ( 'NONE',  ( -1.000000000000000000, -0.000000000000000000, -0.000000000000000000 ) ) ;
#10407 = PRODUCT_DEFINITION_SHAPE ( 'NONE', 'NONE',  #14326 ) ;
#10408 = ORIENTED_EDGE ( 'NONE', *, *, #6997, .F. ) ;
#10409 = ADVANCED_FACE ( 'NONE', ( #3023 ), #6495, .F. ) ;
#10410 = ORIENTED_EDGE ( 'NONE', *, *, #5826, .T. ) ;
#10411 = CARTESIAN_POINT ( 'NONE',  ( 203.5000000000000000, -85.00000000000007105, 180.0000000000000000 ) ) ;
#10412 = CIRCLE ( 'NONE', #3014, 4.250000000000000000 ) ;
#10413 = DIRECTION ( 'NONE',  ( 0.000000000000000000, 0.000000000000000000, 1.000000000000000000 ) ) ;
#10414 = FILL_AREA_STYLE_COLOUR ( '', #7130 ) ;
#10415 = EDGE_LOOP ( 'NONE', ( #9251, #2258, #11399 ) ) ;
#10416 = AXIS2_PLACEMENT_3D ( 'NONE', #1187, #3250, #1997 ) ;
#10417 = B_SPLINE_CURVE_WITH_KNOTS ( 'NONE', 3,
 ( #8034, #4650, #1361, #6815, #189, #10225 ),
 .UNSPECIFIED., .F., .F.,
 ( 4, 2, 4 ),
 ( 0.002452478801916361129, 0.003676905084148001344, 0.004901331366379641126 ),
 .UNSPECIFIED. ) ;
#10418 = DIRECTION ( 'NONE',  ( -0.000000000000000000, -0.000000000000000000, -1.000000000000000000 ) ) ;
#10419 = B_SPLINE_CURVE_WITH_KNOTS ( 'NONE', 3,
 ( #11553, #1601, #12787, #2857, #7269, #11698, #650, #11849 ),
 .UNSPECIFIED., .F., .F.,
 ( 4, 2, 2, 4 ),
 ( 2.465131517071610173E-07, 0.001183067374689837636, 0.001774477805458902699, 0.002365888236227967761 ),
 .UNSPECIFIED. ) ;
#10420 = DIRECTION ( 'NONE',  ( 0.5000000000000022204, 0.8660254037844374864, -0.000000000000000000 ) ) ;
#10421 = DIRECTION ( 'NONE',  ( 0.000000000000000000, 0.000000000000000000, -1.000000000000000000 ) ) ;
#10422 = AXIS2_PLACEMENT_3D ( 'NONE', #11947, #11079, #12226 ) ;
#10423 = DIRECTION ( 'NONE',  ( 0.000000000000000000, -1.000000000000000000, -3.491481338843133355E-15 ) ) ;
#10424 = AXIS2_PLACEMENT_3D ( 'NONE', #5999, #10427, #457 ) ;
#10425 = CIRCLE ( 'NONE', #1138, 2.649999999999985700 ) ;
#10426 = ORIENTED_EDGE ( 'NONE', *, *, #14207, .T. ) ;
#10427 = DIRECTION ( 'NONE',  ( 1.000000000000000000, 0.000000000000000000, 0.000000000000000000 ) ) ;
#10428 = ADVANCED_FACE ( 'NONE', ( #4318 ), #497, .T. ) ;
#10429 = CARTESIAN_POINT ( 'NONE',  ( -2.100000000000000089, 2.571758278209441957E-16, -4.694516984716113228 ) ) ;
#10430 = EDGE_LOOP ( 'NONE', ( #3307, #6186, #14006, #5915 ) ) ;
#10431 = DIRECTION ( 'NONE',  ( -0.000000000000000000, 1.000000000000000000, -0.000000000000000000 ) ) ;
#10432 = CARTESIAN_POINT ( 'NONE',  ( 1.274258131564866448, 3.883108878240963513, -3.220599429844046568 ) ) ;
#10433 = VECTOR ( 'NONE', #8063, 1000.000000000000000 ) ;
#10434 = CARTESIAN_POINT ( 'NONE',  ( 0.06760930072668894231, 0.9010842325122760954, 0.5149999999999993472 ) ) ;
#10435 = DIRECTION ( 'NONE',  ( -0.000000000000000000, -0.000000000000000000, 1.000000000000000000 ) ) ;
#10436 = CARTESIAN_POINT ( 'NONE',  ( 79.99999999999971578, 55.00000000000000711, 0.000000000000000000 ) ) ;
#10437 = CARTESIAN_POINT ( 'NONE',  ( 294.4999999999999432, -95.00000000000008527, -186.2999999999999829 ) ) ;
#10438 = VECTOR ( 'NONE', #11383, 1000.000000000000000 ) ;
#10439 = DIRECTION ( 'NONE',  ( 1.000000000000000000, 0.000000000000000000, 0.000000000000000000 ) ) ;
#10440 = ORIENTED_EDGE ( 'NONE', *, *, #4414, .F. ) ;
#10441 = ORIENTED_EDGE ( 'NONE', *, *, #3477, .F. ) ;
#10442 = DIRECTION ( 'NONE',  ( -0.000000000000000000, -0.000000000000000000, -1.000000000000000000 ) ) ;
#10443 = AXIS2_PLACEMENT_3D ( 'NONE', #10267, #2514, #4760 ) ;
#10444 = EDGE_LOOP ( 'NONE', ( #8181, #10127 ) ) ;
#10445 = CYLINDRICAL_SURFACE ( 'NONE', #4944, 2.500000000000002220 ) ;
#10446 = FACE_OUTER_BOUND ( 'NONE', #2909, .T. ) ;
#10447 = ORIENTED_EDGE ( 'NONE', *, *, #11083, .F. ) ;
#10448 = CARTESIAN_POINT ( 'NONE',  ( -30.00000000000002842, -20.00000000000000000, 240.0000000000000284 ) ) ;
#10449 = EDGE_LOOP ( 'NONE', ( #5107, #10779, #3007, #10759 ) ) ;
#10450 = CIRCLE ( 'NONE', #2349, 2.649999999999985700 ) ;
#10451 = DIRECTION ( 'NONE',  ( 0.000000000000000000, 0.000000000000000000, 1.000000000000000000 ) ) ;
#10452 = CARTESIAN_POINT ( 'NONE',  ( 0.06760930072668806801, -4.837354856632045452E-15, 0.000000000000000000 ) ) ;
#10453 = VERTEX_POINT ( 'NONE', #3243 ) ;
#10454 = PRODUCT_DEFINITION_CONTEXT ( 'detailed design', #13313, 'design' ) ;
#10455 = DIRECTION ( 'NONE',  ( 0.000000000000000000, 0.000000000000000000, -1.000000000000000000 ) ) ;
#10456 = ADVANCED_FACE ( 'NONE', ( #6353 ), #4177, .T. ) ;
#10457 = LINE ( 'NONE', #7974, #2293 ) ;
#10458 = AXIS2_PLACEMENT_3D ( 'NONE', #4108, #12019, #3173 ) ;
#10459 = CARTESIAN_POINT ( 'NONE',  ( -5.000000000000000888, -8.660254037844389075, 205.0000000000000284 ) ) ;
#10460 = APPLICATION_PROTOCOL_DEFINITION ( 'draft international standard', 'automotive_design', 1998, #1355 ) ;
#10461 = CARTESIAN_POINT ( 'NONE',  ( 5.000000000000004441, 0.000000000000000000, 0.000000000000000000 ) ) ;
#10462 = VERTEX_POINT ( 'NONE', #2064 ) ;
#10463 = DIRECTION ( 'NONE',  ( -0.000000000000000000, -0.000000000000000000, -1.000000000000000000 ) ) ;
#10464 = ORIENTED_EDGE ( 'NONE', *, *, #6698, .F. ) ;
#10465 = CARTESIAN_POINT ( 'NONE',  ( 5.000000000000004441, 0.000000000000000000, 4.250000000000000000 ) ) ;
#10466 = CONICAL_SURFACE ( 'NONE', #2597, 2.500000000000002220, 1.029744260000002631 ) ;
#10467 = AXIS2_PLACEMENT_3D ( 'NONE', #3758, #1561, #535 ) ;
#10468 = ORIENTED_EDGE ( 'NONE', *, *, #13753, .F. ) ;
#10469 = DIRECTION ( 'NONE',  ( 0.000000000000000000, 0.000000000000000000, -1.000000000000000000 ) ) ;
#10470 = ORIENTED_EDGE ( 'NONE', *, *, #5826, .F. ) ;
#10471 = CARTESIAN_POINT ( 'NONE',  ( 136.6666666666666288, -20.00000000000000000, -225.1500000000000625 ) ) ;
#10472 = AXIS2_PLACEMENT_3D ( 'NONE', #5497, #8836, #3263 ) ;
#10473 = DIRECTION ( 'NONE',  ( 1.000000000000000000, 0.000000000000000000, 0.000000000000000000 ) ) ;
#10474 = FACE_OUTER_BOUND ( 'NONE', #10806, .T. ) ;
#10475 = EDGE_CURVE ( 'NONE', #7082, #6422, #6333, .T. ) ;
#10476 = PRODUCT_RELATED_PRODUCT_CATEGORY ( 'part', '', ( #4382 ) ) ;
#10477 = CARTESIAN_POINT ( 'NONE',  ( -5.000000000000000888, -8.660254037844389075, 199.9990000000000236 ) ) ;
#10478 = CARTESIAN_POINT ( 'NONE',  ( 0.2500000000000002220, 0.000000000000000000, 0.000000000000000000 ) ) ;
#10479 = CARTESIAN_POINT ( 'NONE',  ( 0.3226060873438244547, -2.189154565102685801, 0.5149999999999992362 ) ) ;
#10480 = TOROIDAL_SURFACE ( 'NONE', #7005, 11.75000000000000000, 1.050000000000000266 ) ;
#10481 = EDGE_LOOP ( 'NONE', ( #9392, #3195, #9029, #4947, #2633, #2497, #8677, #6909 ) ) ;
#10482 = ORIENTED_EDGE ( 'NONE', *, *, #8819, .F. ) ;
#10483 = AXIS2_PLACEMENT_3D ( 'NONE', #11875, #2956, #8382 ) ;
#10484 = STYLED_ITEM ( 'NONE', ( #9108 ), #1760 ) ;
#10485 = AXIS2_PLACEMENT_3D ( 'NONE', #6546, #6613, #12193 ) ;
#10486 = EDGE_CURVE ( 'NONE', #2677, #931, #9626, .T. ) ;
#10487 = ADVANCED_FACE ( 'NONE', ( #11647 ), #14021, .F. ) ;
#10488 =( REPRESENTATION_RELATIONSHIP ('NONE','NONE', #11251, #208 ) REPRESENTATION_RELATIONSHIP_WITH_TRANSFORMATION ( #112 )SHAPE_REPRESENTATION_RELATIONSHIP( ) );
#10489 = ADVANCED_FACE ( 'NONE', ( #1842 ), #13271, .F. ) ;
#10490 = LINE ( 'NONE', #10560, #7434 ) ;
#10491 = CARTESIAN_POINT ( 'NONE',  ( -20.63749999999999929, 0.000000000000000000, 0.000000000000000000 ) ) ;
#10492 = TOROIDAL_SURFACE ( 'NONE', #12580, 2.700000000000000178, 0.2000000000000000111 ) ;
#10493 = EDGE_LOOP ( 'NONE', ( #11397, #424, #11025, #8425 ) ) ;
#10494 = PRODUCT_DEFINITION_FORMATION_WITH_SPECIFIED_SOURCE ( 'ANY', '', #7839, .NOT_KNOWN. ) ;
#10495 = COLOUR_RGB ( '',0.8941176470588234615, 0.8941176470588234615, 0.8941176470588234615 ) ;
#10496 = CARTESIAN_POINT ( 'NONE',  ( -0.2277608394786177770, 0.000000000000000000, 12.77499999999999858 ) ) ;
#10497 = DIRECTION ( 'NONE',  ( 0.000000000000000000, 0.000000000000000000, -1.000000000000000000 ) ) ;
#10498 = DIRECTION ( 'NONE',  ( 6.123233995736766036E-17, 0.000000000000000000, -1.000000000000000000 ) ) ;
#10499 = DIRECTION ( 'NONE',  ( 0.000000000000000000, 1.000000000000000000, 0.000000000000000000 ) ) ;
#10500 = CARTESIAN_POINT ( 'NONE',  ( 347.0000000000000000, -8.660254037844389075, 199.9990000000000236 ) ) ;
#10501 = AXIS2_PLACEMENT_3D ( 'NONE', #13701, #2419, #3840 ) ;
#10502 = ORIENTED_EDGE ( 'NONE', *, *, #10952, .F. ) ;
#10503 = DIRECTION ( 'NONE',  ( -0.000000000000000000, 0.000000000000000000, -1.000000000000000000 ) ) ;
#10504 = ADVANCED_FACE ( 'NONE', ( #11713 ), #2798, .F. ) ;
#10505 = FACE_BOUND ( 'NONE', #5101, .T. ) ;
#10506 = ORIENTED_EDGE ( 'NONE', *, *, #14016, .T. ) ;
#10507 = DIRECTION ( 'NONE',  ( -0.8571673013836870192, 1.049727191973306873E-16, 0.5150380737757234151 ) ) ;
#10508 = CARTESIAN_POINT ( 'NONE',  ( 0.000000000000000000, 0.000000000000000000, 0.000000000000000000 ) ) ;
#10509 = DIRECTION ( 'NONE',  ( -0.000000000000000000, -0.000000000000000000, -1.000000000000000000 ) ) ;
#10510 = CARTESIAN_POINT ( 'NONE',  ( -2.449848172108560540, -3.432307619358754724, -3.503702292528910078 ) ) ;
#10511 = LINE ( 'NONE', #1717, #8387 ) ;
#10512 = CARTESIAN_POINT ( 'NONE',  ( -299.9999999999999432, -75.00000000000008527, 339.9999999999999432 ) ) ;
#10513 =( LENGTH_UNIT ( ) NAMED_UNIT ( * ) SI_UNIT ( .MILLI., .METRE. ) );
#10514 = CARTESIAN_POINT ( 'NONE',  ( -3.436319922987618902, 2.634841920961291439, -3.531542292955721862 ) ) ;
#10515 = CONTEXT_DEPENDENT_SHAPE_REPRESENTATION ( #2332, #13198 ) ;
#10516 = ORIENTED_EDGE ( 'NONE', *, *, #871, .T. ) ;
#10517 = CARTESIAN_POINT ( 'NONE',  ( 197.5000000000000000, -90.00000000000007105, 55.00000000000001421 ) ) ;
#10518 = ORIENTED_EDGE ( 'NONE', *, *, #3507, .F. ) ;
#10519 = CARTESIAN_POINT ( 'NONE',  ( 434.9999999999999432, 8.660254037844390851, 205.0000000000000284 ) ) ;
#10520 = CARTESIAN_POINT ( 'NONE',  ( 2.500000000000000000, -1.178949249685214307, 2.042000000000001592 ) ) ;
#10521 = ORIENTED_EDGE ( 'NONE', *, *, #3925, .F. ) ;
#10522 = DIRECTION ( 'NONE',  ( 1.000000000000000000, 0.000000000000000000, 0.000000000000000000 ) ) ;
#10523 = VERTEX_POINT ( 'NONE', #8520 ) ;
#10524 = CARTESIAN_POINT ( 'NONE',  ( 142.6500000000000057, -95.00000000000008527, -190.0000000000000000 ) ) ;
#10525 = PRODUCT_DEFINITION_SHAPE ( 'NONE', 'NONE',  #14376 ) ;
#10526 = CARTESIAN_POINT ( 'NONE',  ( 2.500000000000000000, 2.357898499370431722, -2.818925648462311528E-15 ) ) ;
#10527 = ORIENTED_EDGE ( 'NONE', *, *, #8747, .F. ) ;
#10528 = SURFACE_SIDE_STYLE ('',( #1663 ) ) ;
#10529 = DIRECTION ( 'NONE',  ( 0.000000000000000000, 0.000000000000000000, -1.000000000000000000 ) ) ;
#10530 = EDGE_CURVE ( 'NONE', #10838, #11122, #8440, .T. ) ;
#10531 = DIRECTION ( 'NONE',  ( 1.000000000000000000, 0.000000000000000000, 0.000000000000000000 ) ) ;
#10532 = APPLICATION_PROTOCOL_DEFINITION ( 'draft international standard', 'automotive_design', 1998, #3874 ) ;
#10533 = DIRECTION ( 'NONE',  ( -0.000000000000000000, -0.000000000000000000, 1.000000000000000000 ) ) ;
#10534 = EDGE_LOOP ( 'NONE', ( #8568, #13933, #350, #13628 ) ) ;
#10535 = VERTEX_POINT ( 'NONE', #4031 ) ;
#10536 = ORIENTED_EDGE ( 'NONE', *, *, #7519, .F. ) ;
#10537 = CLOSED_SHELL ( 'NONE', ( #10428, #10755, #8391, #2400, #1961, #12965, #785, #3018, #4612, #10312, #9891, #14056, #10008, #10065, #3826, #11285, #8522, #10487, #8901, #11357, #5262, #9316, #4510, #7471, #13585, #1679, #7386, #3303 ) ) ;
#10538 = ORIENTED_EDGE ( 'NONE', *, *, #5187, .F. ) ;
#10539 = CARTESIAN_POINT ( 'NONE',  ( 2.500000000000000000, 0.000000000000000000, 0.000000000000000000 ) ) ;
#10540 = EDGE_CURVE ( 'NONE', #678, #6597, #5269, .T. ) ;
#10541 = ORIENTED_EDGE ( 'NONE', *, *, #1089, .T. ) ;
#10542 = CARTESIAN_POINT ( 'NONE',  ( 134.9999999999999716, 45.00000000000001421, 0.000000000000000000 ) ) ;
#10543 = ORIENTED_EDGE ( 'NONE', *, *, #7804, .F. ) ;
#10544 = LINE ( 'NONE', #6260, #134 ) ;
#10545 = CARTESIAN_POINT ( 'NONE',  ( 299.9999999999999432, -75.00000000000008527, 190.0000000000000000 ) ) ;
#10546 = LINE ( 'NONE', #6050, #12201 ) ;
#10547 = APPLICATION_CONTEXT ( 'automotive_design' ) ;
#10548 = FACE_OUTER_BOUND ( 'NONE', #4790, .T. ) ;
#10549 = AXIS2_PLACEMENT_3D ( 'NONE', #7932, #7066, #2430 ) ;
#10550 = FACE_OUTER_BOUND ( 'NONE', #5455, .T. ) ;
#10551 = CARTESIAN_POINT ( 'NONE',  ( 0.000000000000000000, 0.000000000000000000, 0.000000000000000000 ) ) ;
#10552 = ORIENTED_EDGE ( 'NONE', *, *, #238, .F. ) ;
#10553 = ORIENTED_EDGE ( 'NONE', *, *, #10220, .F. ) ;
#10554 = EDGE_CURVE ( 'NONE', #11518, #701, #5853, .T. ) ;
#10555 = DIRECTION ( 'NONE',  ( 0.000000000000000000, 0.000000000000000000, -1.000000000000000000 ) ) ;
#10556 = AXIS2_PLACEMENT_3D ( 'NONE', #2340, #11329, #6759 ) ;
#10557 = EDGE_CURVE ( 'NONE', #10366, #4959, #1696, .T. ) ;
#10558 = VECTOR ( 'NONE', #4273, 1000.000000000000000 ) ;
#10559 = ORIENTED_EDGE ( 'NONE', *, *, #8107, .F. ) ;
#10560 = CARTESIAN_POINT ( 'NONE',  ( 197.5000000000000000, -90.00000000000007105, 50.00000000000001421 ) ) ;
#10561 = LINE ( 'NONE', #5205, #11642 ) ;
#10562 = DIRECTION ( 'NONE',  ( 0.000000000000000000, 0.000000000000000000, 1.000000000000000000 ) ) ;
#10563 = VERTEX_POINT ( 'NONE', #7432 ) ;
#10564 = CARTESIAN_POINT ( 'NONE',  ( -20.63749999999999929, 0.000000000000000000, -10.72500000000000142 ) ) ;
#10565 = EDGE_CURVE ( 'NONE', #13881, #4150, #4099, .T. ) ;
#10566 = AXIS2_PLACEMENT_3D ( 'NONE', #4215, #4283, #14274 ) ;
#10567 = DIRECTION ( 'NONE',  ( 0.000000000000000000, 0.000000000000000000, 1.000000000000000000 ) ) ;
#10568 = CARTESIAN_POINT ( 'NONE',  ( 0.000000000000000000, 0.000000000000000000, 169.9999999999999716 ) ) ;
#10569 = CARTESIAN_POINT ( 'NONE',  ( 2.500000000000000000, 0.000000000000000000, 0.000000000000000000 ) ) ;
#10570 = LINE ( 'NONE', #13894, #12887 ) ;
#10571 = ORIENTED_EDGE ( 'NONE', *, *, #8685, .F. ) ;
#10572 = ADVANCED_FACE ( 'NONE', ( #1987 ), #6421, .F. ) ;
#10573 = CARTESIAN_POINT ( 'NONE',  ( -2.688821387764050996E-14, -4.618802153517012954, -0.4999999999999995559 ) ) ;
#10574 = AXIS2_PLACEMENT_3D ( 'NONE', #2325, #10423, #378 ) ;
#10575 = DIRECTION ( 'NONE',  ( 0.000000000000000000, 0.000000000000000000, -1.000000000000000000 ) ) ;
#10576 = AXIS2_PLACEMENT_3D ( 'NONE', #2933, #5196, #3949 ) ;
#10577 = VERTEX_POINT ( 'NONE', #11937 ) ;
#10578 = CARTESIAN_POINT ( 'NONE',  ( -5.000000000000000888, -8.660254037844389075, 200.0000000000000000 ) ) ;
#10579 = AXIS2_PLACEMENT_3D ( 'NONE', #1388, #2711, #10469 ) ;
#10580 =( NAMED_UNIT ( * ) PLANE_ANGLE_UNIT ( ) SI_UNIT ( $, .RADIAN. ) );
#10581 = EDGE_CURVE ( 'NONE', #4302, #4187, #3541, .T. ) ;
#10582 = CARTESIAN_POINT ( 'NONE',  ( -0.6920835326022555245, -4.454600218803899558, -3.597382984111586079 ) ) ;
#10583 = LINE ( 'NONE', #1494, #9322 ) ;
#10584 = DIRECTION ( 'NONE',  ( 0.000000000000000000, -0.5000000000000012212, -0.8660254037844380415 ) ) ;
#10585 =( NAMED_UNIT ( * ) PLANE_ANGLE_UNIT ( ) SI_UNIT ( $, .RADIAN. ) );
#10586 = VECTOR ( 'NONE', #4861, 1000.000000000000000 ) ;
#10587 = EDGE_CURVE ( 'NONE', #4143, #7082, #43, .T. ) ;
#10588 = CARTESIAN_POINT ( 'NONE',  ( 0.1404048886732821022, 4.699864953788070565, -3.686887068327037387 ) ) ;
#10589 = AXIS2_PLACEMENT_3D ( 'NONE', #8305, #8224, #7149 ) ;
#10590 = CIRCLE ( 'NONE', #9428, 2.649999999999985700 ) ;
#10591 = ORIENTED_EDGE ( 'NONE', *, *, #716, .T. ) ;
#10592 = EDGE_CURVE ( 'NONE', #11555, #9162, #1675, .T. ) ;
#10593 = CIRCLE ( 'NONE', #128, 0.2500000000000002220 ) ;
#10594 = PLANE ( 'NONE',  #10310 ) ;
#10595 = AXIS2_PLACEMENT_3D ( 'NONE', #656, #2048, #8582 ) ;
#10596 = VERTEX_POINT ( 'NONE', #588 ) ;
#10597 = CARTESIAN_POINT ( 'NONE',  ( 219.9999999999999716, -85.00000000000007105, 170.0000000000000000 ) ) ;
#10598 = DIRECTION ( 'NONE',  ( -0.000000000000000000, -0.000000000000000000, 1.000000000000000000 ) ) ;
#10599 = VECTOR ( 'NONE', #9153, 1000.000000000000000 ) ;
#10600 = EDGE_LOOP ( 'NONE', ( #5248, #12531, #13789, #11457 ) ) ;
#10601 = CARTESIAN_POINT ( 'NONE',  ( 137.4999999999999716, 45.00000000000001421, 0.000000000000000000 ) ) ;
#10602 = VERTEX_POINT ( 'NONE', #9469 ) ;
#10603 = DIRECTION ( 'NONE',  ( -0.000000000000000000, -0.000000000000000000, 1.000000000000000000 ) ) ;
#10604 = AXIS2_PLACEMENT_3D ( 'NONE', #9009, #5606, #11257 ) ;
#10605 = CARTESIAN_POINT ( 'NONE',  ( 0.000000000000000000, 0.000000000000000000, -190.0000000000000000 ) ) ;
#10606 = ORIENTED_EDGE ( 'NONE', *, *, #3580, .T. ) ;
#10607 = CARTESIAN_POINT ( 'NONE',  ( -5.000000000000000888, -8.660254037844389075, -200.0000000000000284 ) ) ;
#10608 = VECTOR ( 'NONE', #11294, 1000.000000000000000 ) ;
#10609 = DIRECTION ( 'NONE',  ( 1.000000000000000000, 0.000000000000000000, -0.000000000000000000 ) ) ;
#10610 = AXIS2_PLACEMENT_3D ( 'NONE', #9441, #11684, #850 ) ;
#10611 = FACE_OUTER_BOUND ( 'NONE', #10061, .T. ) ;
#10612 = PRODUCT_CONTEXT ( 'NONE', #605, 'mechanical' ) ;
#10613 = DIRECTION ( 'NONE',  ( 1.000000000000000000, 0.000000000000000000, 0.000000000000000000 ) ) ;
#10614 = AXIS2_PLACEMENT_3D ( 'NONE', #9304, #13717, #3790 ) ;
#10615 = VERTEX_POINT ( 'NONE', #1920 ) ;
#10616 = EDGE_LOOP ( 'NONE', ( #2185, #9267, #8557, #13119 ) ) ;
#10617 = CARTESIAN_POINT ( 'NONE',  ( 5.384454397937118664, 0.000000000000000000, -5.000000000000000000 ) ) ;
#10618 = EDGE_LOOP ( 'NONE', ( #1083, #8352, #6946, #10667 ) ) ;
#10619 = LINE ( 'NONE', #1678, #2139 ) ;
#10620 = AXIS2_PLACEMENT_3D ( 'NONE', #12365, #11072, #5625 ) ;
#10621 = EDGE_CURVE ( 'NONE', #2327, #8720, #9693, .T. ) ;
#10622 = EDGE_LOOP ( 'NONE', ( #724, #3001, #10330, #12245 ) ) ;
#10623 = DIRECTION ( 'NONE',  ( -1.000000000000000000, -0.000000000000000000, -0.000000000000000000 ) ) ;
#10624 = ORIENTED_EDGE ( 'NONE', *, *, #3848, .F. ) ;
#10625 = CARTESIAN_POINT ( 'NONE',  ( 2.500000000000000000, 0.000000000000000000, 0.000000000000000000 ) ) ;
#10626 = CARTESIAN_POINT ( 'NONE',  ( 4.999999999999999112, 8.660254037844390851, 210.0000000000000000 ) ) ;
#10627 = DIRECTION ( 'NONE',  ( 1.000000000000000000, 0.000000000000000000, 0.000000000000000000 ) ) ;
#10628 = CARTESIAN_POINT ( 'NONE',  ( -299.9999999999999432, -75.00000000000008527, 0.000000000000000000 ) ) ;
#10629 = FILL_AREA_STYLE_COLOUR ( '', #2103 ) ;
#10630 = AXIS2_PLACEMENT_3D ( 'NONE', #10545, #5832, #577 ) ;
#10631 = LINE ( 'NONE', #4971, #12244 ) ;
#10632 = ORIENTED_EDGE ( 'NONE', *, *, #7073, .T. ) ;
#10633 = ORIENTED_EDGE ( 'NONE', *, *, #6816, .T. ) ;
#10634 = CARTESIAN_POINT ( 'NONE',  ( -31.74999999999995737, 0.000000000000000000, 2.500000000000000444 ) ) ;
#10635 = EDGE_CURVE ( 'NONE', #11495, #1881, #3331, .T. ) ;
#10636 = LINE ( 'NONE', #668, #8238 ) ;
#10637 = CIRCLE ( 'NONE', #13863, 2.649999999999985700 ) ;
#10638 = CARTESIAN_POINT ( 'NONE',  ( 2.500000000000000000, -2.357898499370432610, 3.252606517456513302E-15 ) ) ;
#10639 = CARTESIAN_POINT ( 'NONE',  ( 299.9999999999999432, -95.00000000000008527, -169.9999999999999716 ) ) ;
#10640 = ORIENTED_EDGE ( 'NONE', *, *, #4457, .T. ) ;
#10641 = AXIS2_PLACEMENT_3D ( 'NONE', #4506, #9948, #10080 ) ;
#10642 = CARTESIAN_POINT ( 'NONE',  ( 2.500000000000000000, 1.178949249685212974, -2.042000000000001148 ) ) ;
#10643 = ADVANCED_FACE ( 'NONE', ( #13882 ), #8372, .T. ) ;
#10644 = CYLINDRICAL_SURFACE ( 'NONE', #2304, 4.250000000000000000 ) ;
#10645 = DIRECTION ( 'NONE',  ( 6.123233995736766036E-17, 0.000000000000000000, 1.000000000000000000 ) ) ;
#10646 = ADVANCED_FACE ( 'NONE', ( #1022 ), #2135, .T. ) ;
#10647 = CARTESIAN_POINT ( 'NONE',  ( -4.000000000000000000, -2.309401076758515803, -0.4999999999999995559 ) ) ;
#10648 = EDGE_LOOP ( 'NONE', ( #5735, #8594 ) ) ;
#10649 = CIRCLE ( 'NONE', #12959, 2.649999999999985700 ) ;
#10650 = CARTESIAN_POINT ( 'NONE',  ( 24.55500000000002103, 0.000000000000000000, 2.500000000000001332 ) ) ;
#10651 = PRODUCT_DEFINITION_SHAPE ( 'NONE', 'NONE',  #14345 ) ;
#10652 = FACE_OUTER_BOUND ( 'NONE', #7, .T. ) ;
#10653 = VERTEX_POINT ( 'NONE', #6566 ) ;
#10654 = CARTESIAN_POINT ( 'NONE',  ( 17.00000000000000000, 2.516649172247811061E-16, -2.055000000000000160 ) ) ;
#10655 = FILL_AREA_STYLE_COLOUR ( '', #26 ) ;
#10656 = CARTESIAN_POINT ( 'NONE',  ( 203.5000000000000000, -85.00000000000007105, 180.0000000000000000 ) ) ;
#10657 = CIRCLE ( 'NONE', #6252, 2.649999999999985700 ) ;
#10658 = EDGE_CURVE ( 'NONE', #1127, #2208, #5405, .T. ) ;
#10659 = CARTESIAN_POINT ( 'NONE',  ( 305.4999999999999432, -75.00000000000008527, -186.2999999999999829 ) ) ;
#10660 = EDGE_CURVE ( 'NONE', #11926, #5030, #8880, .T. ) ;
#10661 = CARTESIAN_POINT ( 'NONE',  ( -4.000000000000000000, 0.000000000000000000, 0.000000000000000000 ) ) ;
#10662 = CARTESIAN_POINT ( 'NONE',  ( 0.000000000000000000, 0.000000000000000000, 0.000000000000000000 ) ) ;
#10663 = CIRCLE ( 'NONE', #5856, 2.649999999999985700 ) ;
#10664 = CARTESIAN_POINT ( 'NONE',  ( 219.9999999999999716, -20.00000000000000000, 222.5000000000000853 ) ) ;
#10665 = ORIENTED_EDGE ( 'NONE', *, *, #13504, .T. ) ;
#10666 = CARTESIAN_POINT ( 'NONE',  ( 13.50000000000000000, 1.653273178848926867E-15, -186.0000000000000000 ) ) ;
#10667 = ORIENTED_EDGE ( 'NONE', *, *, #10143, .T. ) ;
#10668 = DIRECTION ( 'NONE',  ( -1.000000000000000000, 0.000000000000000000, 0.000000000000000000 ) ) ;
#10669 = LINE ( 'NONE', #9582, #12574 ) ;
#10670 = EDGE_CURVE ( 'NONE', #5183, #2298, #4462, .T. ) ;
#10671 = EDGE_CURVE ( 'NONE', #3349, #1111, #7776, .T. ) ;
#10672 = VECTOR ( 'NONE', #2219, 1000.000000000000000 ) ;
#10673 = VERTEX_POINT ( 'NONE', #9977 ) ;
#10674 = EDGE_CURVE ( 'NONE', #9002, #10602, #12011, .T. ) ;
#10675 = CYLINDRICAL_SURFACE ( 'NONE', #8748, 2.500000000000002220 ) ;
#10676 = VERTEX_POINT ( 'NONE', #1099 ) ;
#10677 = DIRECTION ( 'NONE',  ( 0.000000000000000000, -0.000000000000000000, 1.000000000000000000 ) ) ;
#10678 = ORIENTED_EDGE ( 'NONE', *, *, #9973, .T. ) ;
#10679 = VECTOR ( 'NONE', #5153, 1000.000000000000114 ) ;
#10680 = CARTESIAN_POINT ( 'NONE',  ( 470.0000000000000000, 15.00000000000000000, 205.0000000000000284 ) ) ;
#10681 = CARTESIAN_POINT ( 'NONE',  ( 140.0000000000000000, -75.00000000000008527, -190.0000000000000000 ) ) ;
#10682 = ITEM_DEFINED_TRANSFORMATION ( 'NONE', 'NONE', #5610,  #14039 ) ;
#10683 = CARTESIAN_POINT ( 'NONE',  ( -20.63749999999999574, 0.000000000000000000, -12.77499999999999858 ) ) ;
#10684 = AXIS2_PLACEMENT_3D ( 'NONE', #10411, #2583, #13596 ) ;
#10685 = VERTEX_POINT ( 'NONE', #1245 ) ;
#10686 =( REPRESENTATION_RELATIONSHIP ('NONE','NONE', #11251, #13104 ) REPRESENTATION_RELATIONSHIP_WITH_TRANSFORMATION ( #1571 )SHAPE_REPRESENTATION_RELATIONSHIP( ) );
#10687 = EDGE_LOOP ( 'NONE', ( #1702, #7050 ) ) ;
#10688 = VERTEX_POINT ( 'NONE', #5468 ) ;
#10689 = VERTEX_POINT ( 'NONE', #7572 ) ;
#10690 = VECTOR ( 'NONE', #5629, 1000.000000000000114 ) ;
#10691 = DIRECTION ( 'NONE',  ( 0.000000000000000000, 0.000000000000000000, 1.000000000000000000 ) ) ;
#10692 = ORIENTED_EDGE ( 'NONE', *, *, #10486, .T. ) ;
#10693 = ORIENTED_EDGE ( 'NONE', *, *, #12000, .T. ) ;
#10694 = DIRECTION ( 'NONE',  ( 0.000000000000000000, 0.000000000000000000, 1.000000000000000000 ) ) ;
#10695 = EDGE_LOOP ( 'NONE', ( #8200, #845 ) ) ;
#10696 = CARTESIAN_POINT ( 'NONE',  ( -299.9999999999999432, -75.00000000000008527, 0.000000000000000000 ) ) ;
#10697 = UNCERTAINTY_MEASURE_WITH_UNIT (LENGTH_MEASURE( 1.000000000000000082E-05 ), #659, 'distance_accuracy_value', 'NONE');
#10698 = DIRECTION ( 'NONE',  ( -0.000000000000000000, -0.000000000000000000, -1.000000000000000000 ) ) ;
#10699 = DIRECTION ( 'NONE',  ( 0.000000000000000000, 1.000000000000000000, 0.000000000000000000 ) ) ;
#10700 = DIRECTION ( 'NONE',  ( 0.000000000000000000, 0.000000000000000000, 1.000000000000000000 ) ) ;
#10701 = VECTOR ( 'NONE', #5744, 1000.000000000000000 ) ;
#10702 = SURFACE_SIDE_STYLE ('',( #11933 ) ) ;
#10703 = FACE_OUTER_BOUND ( 'NONE', #2184, .T. ) ;
#10704 = ORIENTED_EDGE ( 'NONE', *, *, #5765, .T. ) ;
#10705 = EDGE_CURVE ( 'NONE', #2464, #806, #2060, .T. ) ;
#10706 = ORIENTED_EDGE ( 'NONE', *, *, #10660, .T. ) ;
#10707 = CIRCLE ( 'NONE', #2363, 2.500000000000000888 ) ;
#10708 = CARTESIAN_POINT ( 'NONE',  ( 5.200000000000002842, 0.000000000000000000, -2.700000000000000622 ) ) ;
#10709 = COLOUR_RGB ( '',1.000000000000000000, 0.9490196078431372140, 0.9098039215686274384 ) ;
#10710 = ORIENTED_EDGE ( 'NONE', *, *, #5055, .T. ) ;
#10711 = CARTESIAN_POINT ( 'NONE',  ( 3.900000000000000799, 3.061616997868383141E-16, -2.500000000000000000 ) ) ;
#10712 = FACE_OUTER_BOUND ( 'NONE', #7763, .T. ) ;
#10713 = SHAPE_REPRESENTATION ( 'vertical suport', ( #14039 ), #3056 ) ;
#10714 = DIRECTION ( 'NONE',  ( -0.000000000000000000, 0.000000000000000000, 1.000000000000000000 ) ) ;
#10715 = B_SPLINE_CURVE_WITH_KNOTS ( 'NONE', 3,
 ( #13103, #14051, #3045, #14261, #975 ),
 .UNSPECIFIED., .F., .F.,
 ( 4, 1, 4 ),
 ( 5.640274452250024914E-20, 0.002309401076758505356, 0.004618802153517010713 ),
 .UNSPECIFIED. ) ;
#10716 = ORIENTED_EDGE ( 'NONE', *, *, #9788, .T. ) ;
#10717 = AXIS2_PLACEMENT_3D ( 'NONE', #8990, #185, #11172 ) ;
#10718 = DIRECTION ( 'NONE',  ( -0.000000000000000000, -0.000000000000000000, 1.000000000000000000 ) ) ;
#10719 = AXIS2_PLACEMENT_3D ( 'NONE', #11437, #13604, #10202 ) ;
#10720 = DIRECTION ( 'NONE',  ( -0.000000000000000000, -0.000000000000000000, 1.000000000000000000 ) ) ;
#10721 = CARTESIAN_POINT ( 'NONE',  ( 219.9999999999999147, -85.00000000000009948, 125.0000000000000000 ) ) ;
#10722 = LINE ( 'NONE', #9625, #7640 ) ;
#10723 = CONICAL_SURFACE ( 'NONE', #1198, 2.055000000000000160, 0.7853981633974721488 ) ;
#10724 = EDGE_LOOP ( 'NONE', ( #4336, #12334, #13990, #2528, #4875 ) ) ;
#10725 = ORIENTED_EDGE ( 'NONE', *, *, #12585, .T. ) ;
#10726 = DIRECTION ( 'NONE',  ( 0.000000000000000000, 0.000000000000000000, 1.000000000000000000 ) ) ;
#10727 = AXIS2_PLACEMENT_3D ( 'NONE', #10125, #12516, #4761 ) ;
#10728 = LINE ( 'NONE', #3038, #5805 ) ;
#10729 = EDGE_CURVE ( 'NONE', #10177, #13284, #9902, .T. ) ;
#10730 = ADVANCED_FACE ( 'NONE', ( #1278 ), #13688, .T. ) ;
#10731 = ORIENTED_EDGE ( 'NONE', *, *, #7916, .T. ) ;
#10732 = AXIS2_PLACEMENT_3D ( 'NONE', #2757, #3919, #5090 ) ;
#10733 = EDGE_CURVE ( 'NONE', #8663, #4316, #8811, .T. ) ;
#10734 = CARTESIAN_POINT ( 'NONE',  ( 2.059999999999998721, 0.000000000000000000, -0.3080913168122742518 ) ) ;
#10735 =( NAMED_UNIT ( * ) SI_UNIT ( $, .STERADIAN. ) SOLID_ANGLE_UNIT ( ) );
#10736 = CARTESIAN_POINT ( 'NONE',  ( 2.500000000000000000, 2.357898499370433054, -1.951563910473907981E-15 ) ) ;
#10737 = CIRCLE ( 'NONE', #10030, 2.649999999999985700 ) ;
#10738 = EDGE_LOOP ( 'NONE', ( #4011, #10229, #12819, #6807 ) ) ;
#10739 = DIRECTION ( 'NONE',  ( -1.000000000000000000, 0.000000000000000000, 0.000000000000000000 ) ) ;
#10740 = ORIENTED_EDGE ( 'NONE', *, *, #5173, .T. ) ;
#10741 = CARTESIAN_POINT ( 'NONE',  ( -140.0000000000000000, -75.00000000000008527, 40.00000000000000000 ) ) ;
#10742 = CYLINDRICAL_SURFACE ( 'NONE', #6324, 12.00000000000000000 ) ;
#10743 = EDGE_CURVE ( 'NONE', #67, #7902, #2280, .T. ) ;
#10744 = PRODUCT_RELATED_PRODUCT_CATEGORY ( 'part', '', ( #4495 ) ) ;
#10745 = ORIENTED_EDGE ( 'NONE', *, *, #7189, .F. ) ;
#10746 = CARTESIAN_POINT ( 'NONE',  ( -3.511755186886750479, 2.826662030176366081, -3.597382984111578086 ) ) ;
#10747 = ORIENTED_EDGE ( 'NONE', *, *, #12534, .F. ) ;
#10748 = CARTESIAN_POINT ( 'NONE',  ( -135.0000000000000000, -75.00000000000008527, 30.00000000000000000 ) ) ;
#10749 = DIRECTION ( 'NONE',  ( -0.000000000000000000, -0.000000000000000000, -1.000000000000000000 ) ) ;
#10750 = ORIENTED_EDGE ( 'NONE', *, *, #5512, .T. ) ;
#10751 = SURFACE_STYLE_USAGE ( .BOTH. , #5172 ) ;
#10752 = DIRECTION ( 'NONE',  ( -0.000000000000000000, -0.000000000000000000, -1.000000000000000000 ) ) ;
#10753 =( NAMED_UNIT ( * ) SI_UNIT ( $, .STERADIAN. ) SOLID_ANGLE_UNIT ( ) );
#10754 = FILL_AREA_STYLE ('',( #642 ) ) ;
#10755 = ADVANCED_FACE ( 'NONE', ( #10919 ), #3165, .T. ) ;
#10756 = EDGE_CURVE ( 'NONE', #10395, #11926, #1915, .T. ) ;
#10757 = DIRECTION ( 'NONE',  ( 1.000000000000000000, 0.000000000000000000, 0.000000000000000000 ) ) ;
#10758 = ORIENTED_EDGE ( 'NONE', *, *, #3404, .T. ) ;
#10759 = ORIENTED_EDGE ( 'NONE', *, *, #10540, .F. ) ;
#10760 = LINE ( 'NONE', #8571, #11228 ) ;
#10761 = ORIENTED_EDGE ( 'NONE', *, *, #10853, .T. ) ;
#10762 = CARTESIAN_POINT ( 'NONE',  ( 134.5000000000000000, -75.00000000000008527, -190.0000000000000000 ) ) ;
#10763 = EDGE_CURVE ( 'NONE', #13552, #7639, #10737, .T. ) ;
#10764 = EDGE_LOOP ( 'NONE', ( #4746, #1526, #10376, #13065, #2562 ) ) ;
#10765 = ORIENTED_EDGE ( 'NONE', *, *, #10370, .T. ) ;
#10766 = CARTESIAN_POINT ( 'NONE',  ( -124.9999999999999432, -105.0000000000000853, 40.00000000000000000 ) ) ;
#10767 = EDGE_LOOP ( 'NONE', ( #12989, #5785, #9812 ) ) ;
#10768 = DIRECTION ( 'NONE',  ( -1.000000000000000000, -0.000000000000000000, -0.000000000000000000 ) ) ;
#10769 = CARTESIAN_POINT ( 'NONE',  ( 299.9999999999999432, -95.00000000000008527, -186.2999999999999829 ) ) ;
#10770 = LINE ( 'NONE', #4384, #8745 ) ;
#10771 =( REPRESENTATION_RELATIONSHIP ('NONE','NONE', #11251, #3385 ) REPRESENTATION_RELATIONSHIP_WITH_TRANSFORMATION ( #2088 )SHAPE_REPRESENTATION_RELATIONSHIP( ) );
#10772 = DIRECTION ( 'NONE',  ( -0.000000000000000000, -0.000000000000000000, 1.000000000000000000 ) ) ;
#10773 = ADVANCED_FACE ( 'NONE', ( #12212 ), #13364, .T. ) ;
#10774 = CARTESIAN_POINT ( 'NONE',  ( 4.000000000000000000, -2.309401076758514915, -3.433295621305383349 ) ) ;
#10775 = PRODUCT_DEFINITION_SHAPE ( 'NONE', 'NONE',  #14343 ) ;
#10776 = CIRCLE ( 'NONE', #1019, 2.500000000000000888 ) ;
#10777 = ORIENTED_EDGE ( 'NONE', *, *, #8449, .F. ) ;
#10778 = ADVANCED_FACE ( 'NONE', ( #10045 ), #9333, .F. ) ;
#10779 = ORIENTED_EDGE ( 'NONE', *, *, #13637, .T. ) ;
#10780 = EDGE_CURVE ( 'NONE', #1682, #1365, #4250, .T. ) ;
#10781 = DIRECTION ( 'NONE',  ( 0.000000000000000000, -0.000000000000000000, 1.000000000000000000 ) ) ;
#10782 = DIRECTION ( 'NONE',  ( 1.000000000000000000, 0.000000000000000000, 0.000000000000000000 ) ) ;
#10783 = CARTESIAN_POINT ( 'NONE',  ( -135.0000000000000000, -95.00000000000008527, -14.14213562373090127 ) ) ;
#10784 = VECTOR ( 'NONE', #12401, 1000.000000000000000 ) ;
#10785 = CARTESIAN_POINT ( 'NONE',  ( -30.00000000000002842, -225.0000000000000000, -169.9999999999999716 ) ) ;
#10786 = AXIS2_PLACEMENT_3D ( 'NONE', #3371, #12204, #7633 ) ;
#10787 = EDGE_LOOP ( 'NONE', ( #10518, #5227, #3626, #10624 ) ) ;
#10788 = DIRECTION ( 'NONE',  ( -0.000000000000000000, -0.000000000000000000, 1.000000000000000000 ) ) ;
#10789 = CARTESIAN_POINT ( 'NONE',  ( 5.000000000000000888, 0.000000000000000000, 0.000000000000000000 ) ) ;
#10790 = CARTESIAN_POINT ( 'NONE',  ( 386.6666666666666288, -30.00000000000000355, -222.5000000000000853 ) ) ;
#10791 = DIRECTION ( 'NONE',  ( 0.000000000000000000, 0.000000000000000000, 1.000000000000000000 ) ) ;
#10792 = EDGE_LOOP ( 'NONE', ( #12499, #4889 ) ) ;
#10793 = AXIS2_PLACEMENT_3D ( 'NONE', #1873, #7461, #6303 ) ;
#10794 = ORIENTED_EDGE ( 'NONE', *, *, #10110, .T. ) ;
#10795 = CARTESIAN_POINT ( 'NONE',  ( 203.5000000000000000, -85.00000000000007105, 190.0000000000000000 ) ) ;
#10796 = SHAPE_REPRESENTATION ( 'socket head cap screw_iso_ISO 4762 M5 x 12 - 12N', ( #14039 ), #3976 ) ;
#10797 = CARTESIAN_POINT ( 'NONE',  ( 0.9586399445693630783, 0.5150000000000030109, -0.8293189044373061591 ) ) ;
#10798 = EDGE_CURVE ( 'NONE', #10296, #6403, #11188, .T. ) ;
#10799 = EDGE_LOOP ( 'NONE', ( #6669, #4950, #973, #6126 ) ) ;
#10800 = LINE ( 'NONE', #12824, #9888 ) ;
#10801 = VECTOR ( 'NONE', #1011, 1000.000000000000341 ) ;
#10802 = CARTESIAN_POINT ( 'NONE',  ( -30.00000000000002842, -25.00000000000000000, 250.0000000000000000 ) ) ;
#10803 = CARTESIAN_POINT ( 'NONE',  ( 4.211405965630455661, 2.460463115436283932, -3.751298928144577882 ) ) ;
#10804 = DIRECTION ( 'NONE',  ( 1.000000000000000000, 0.000000000000000000, 0.000000000000000000 ) ) ;
#10805 = ITEM_DEFINED_TRANSFORMATION ( 'NONE', 'NONE', #1196,  #14039 ) ;
#10806 = EDGE_LOOP ( 'NONE', ( #8699, #2201, #5355 ) ) ;
#10807 = CARTESIAN_POINT ( 'NONE',  ( 181.0000000000000000, 8.660254037844390851, 205.0000000000000284 ) ) ;
#10808 = VECTOR ( 'NONE', #10507, 1000.000000000000000 ) ;
#10809 = VERTEX_POINT ( 'NONE', #13436 ) ;
#10810 = CARTESIAN_POINT ( 'NONE',  ( -25.39999999999996305, 0.000000000000000000, 0.000000000000000000 ) ) ;
#10811 = LINE ( 'NONE', #9648, #2792 ) ;
#10812 = AXIS2_PLACEMENT_3D ( 'NONE', #11417, #5828, #3655 ) ;
#10813 = ORIENTED_EDGE ( 'NONE', *, *, #6848, .F. ) ;
#10814 = CARTESIAN_POINT ( 'NONE',  ( -2.805705207896067144, 3.226868319750155312, -3.503898532754364581 ) ) ;
#10815 = ORIENTED_EDGE ( 'NONE', *, *, #4097, .F. ) ;
#10816 = CARTESIAN_POINT ( 'NONE',  ( 219.9999999999999716, -14.99999999999999822, 225.1500000000000625 ) ) ;
#10817 = CARTESIAN_POINT ( 'NONE',  ( -4.000000000000000000, 1.941961291383472732, -0.3515519931180205448 ) ) ;
#10818 = ORIENTED_EDGE ( 'NONE', *, *, #1970, .F. ) ;
#10819 = CIRCLE ( 'NONE', #12653, 2.649999999999985700 ) ;
#10820 = CARTESIAN_POINT ( 'NONE',  ( 0.000000000000000000, 0.000000000000000000, -4.484454397937119197 ) ) ;
#10821 = CARTESIAN_POINT ( 'NONE',  ( -31.74999999999995737, 0.000000000000000000, 0.000000000000000000 ) ) ;
#10822 = AXIS2_PLACEMENT_3D ( 'NONE', #8613, #831, #13901 ) ;
#10823 = FACE_BOUND ( 'NONE', #5343, .T. ) ;
#10824 = EDGE_CURVE ( 'NONE', #13895, #140, #2904, .T. ) ;
#10825 = VECTOR ( 'NONE', #10623, 1000.000000000000000 ) ;
#10826 = DIRECTION ( 'NONE',  ( 0.000000000000000000, 0.000000000000000000, 1.000000000000000000 ) ) ;
#10827 = ADVANCED_FACE ( 'NONE', ( #3516 ), #8185, .F. ) ;
#10828 = ORIENTED_EDGE ( 'NONE', *, *, #10049, .T. ) ;
#10829 = ORIENTED_EDGE ( 'NONE', *, *, #2595, .F. ) ;
#10830 = DIRECTION ( 'NONE',  ( 0.4461977533474923430, 3.124646727056501411E-15, -0.8949343913984144638 ) ) ;
#10831 = VECTOR ( 'NONE', #575, 1000.000000000000000 ) ;
#10832 = ORIENTED_EDGE ( 'NONE', *, *, #12797, .T. ) ;
#10833 = DIRECTION ( 'NONE',  ( -1.000000000000000000, 0.000000000000000000, 0.000000000000000000 ) ) ;
#10834 = EDGE_LOOP ( 'NONE', ( #9817, #13507, #11652, #11928, #6361 ) ) ;
#10835 = CIRCLE ( 'NONE', #1540, 7.983406227920510467 ) ;
#10836 = ORIENTED_EDGE ( 'NONE', *, *, #1331, .F. ) ;
#10837 = DIRECTION ( 'NONE',  ( 1.000000000000000000, 0.000000000000000000, 0.000000000000000000 ) ) ;
#10838 = VERTEX_POINT ( 'NONE', #2834 ) ;
#10839 = DIRECTION ( 'NONE',  ( -1.000000000000000000, 0.000000000000000000, 0.000000000000000000 ) ) ;
#10840 = VECTOR ( 'NONE', #11253, 1000.000000000000000 ) ;
#10841 = AXIS2_PLACEMENT_3D ( 'NONE', #6619, #9008, #7840 ) ;
#10842 = CARTESIAN_POINT ( 'NONE',  ( 299.9999999999999432, -75.00000000000008527, -190.0000000000000000 ) ) ;
#10843 = DIRECTION ( 'NONE',  ( 0.000000000000000000, -1.000000000000000000, 0.000000000000000000 ) ) ;
#10844 = AXIS2_PLACEMENT_3D ( 'NONE', #13156, #11060, #3373 ) ;
#10845 = CYLINDRICAL_SURFACE ( 'NONE', #228, 2.649999999999985700 ) ;
#10846 = ADVANCED_FACE ( 'NONE', ( #9362 ), #10445, .F. ) ;
#10847 = ADVANCED_FACE ( 'NONE', ( #630 ), #12688, .F. ) ;
#10848 = COLOUR_RGB ( '',1.000000000000000000, 0.9490196078431372140, 0.9098039215686274384 ) ;
#10849 = CARTESIAN_POINT ( 'NONE',  ( 136.6666666666666288, -25.00000000000000000, -222.5000000000000853 ) ) ;
#10850 = ORIENTED_EDGE ( 'NONE', *, *, #3117, .T. ) ;
#10851=STYLED_ITEM('',(#14417),#13134);
#10852 = ORIENTED_EDGE ( 'NONE', *, *, #12960, .T. ) ;
#10853 = EDGE_CURVE ( 'NONE', #7714, #4256, #11269, .T. ) ;
#10854 = DIRECTION ( 'NONE',  ( 1.000000000000000000, 0.000000000000000000, 0.000000000000000000 ) ) ;
#10855 = EDGE_LOOP ( 'NONE', ( #10033, #9019 ) ) ;
#10856 = CARTESIAN_POINT ( 'NONE',  ( 140.0000000000000000, -75.00000000000008527, -169.9999999999999716 ) ) ;
#10857 = CARTESIAN_POINT ( 'NONE',  ( 5.200000000000002842, 0.000000000000000000, 0.000000000000000000 ) ) ;
#10858 = EDGE_CURVE ( 'NONE', #8006, #11938, #4675, .T. ) ;
#10859 = EDGE_CURVE ( 'NONE', #1275, #4230, #14197, .T. ) ;
#10860 = ORIENTED_EDGE ( 'NONE', *, *, #5239, .T. ) ;
#10861 = EDGE_CURVE ( 'NONE', #12703, #791, #509, .T. ) ;
#10862 = VECTOR ( 'NONE', #4035, 1000.000000000000000 ) ;
#10863 = FACE_OUTER_BOUND ( 'NONE', #11182, .T. ) ;
#10864 = LINE ( 'NONE', #888, #5779 ) ;
#10865 = CARTESIAN_POINT ( 'NONE',  ( 28.70000000000000284, 0.000000000000000000, 2.500000000000000000 ) ) ;
#10866 = AXIS2_PLACEMENT_3D ( 'NONE', #10821, #8566, #3066 ) ;
#10867 = VERTEX_POINT ( 'NONE', #5089 ) ;
#10868 = ORIENTED_EDGE ( 'NONE', *, *, #3527, .F. ) ;
#10869 = CARTESIAN_POINT ( 'NONE',  ( 219.9999999999999716, -85.00000000000007105, 50.00000000000001421 ) ) ;
#10870 = CARTESIAN_POINT ( 'NONE',  ( 2.740000000000000213, 0.5150000000000024558, -0.6774776749089207462 ) ) ;
#10871 = VECTOR ( 'NONE', #9640, 1000.000000000000000 ) ;
#10872 = ORIENTED_EDGE ( 'NONE', *, *, #10756, .F. ) ;
#10873 = CARTESIAN_POINT ( 'NONE',  ( 0.2500000000000002220, 0.000000000000000000, 4.000000000000000000 ) ) ;
#10874 = AXIS2_PLACEMENT_3D ( 'NONE', #12117, #1065, #8923 ) ;
#10875 = DIRECTION ( 'NONE',  ( 0.000000000000000000, -1.000000000000000000, 0.000000000000000000 ) ) ;
#10876 = CARTESIAN_POINT ( 'NONE',  ( -1.799999999999996048, 0.000000000000000000, -9.999999999999998224 ) ) ;
#10877 = VECTOR ( 'NONE', #12660, 1000.000000000000114 ) ;
#10878 = ITEM_DEFINED_TRANSFORMATION ( 'NONE', 'NONE', #4239,  #14039 ) ;
#10879 = EDGE_CURVE ( 'NONE', #2998, #12823, #13733, .T. ) ;
#10880 = ORIENTED_EDGE ( 'NONE', *, *, #8818, .F. ) ;
#10881 = DIRECTION ( 'NONE',  ( -0.000000000000000000, -0.000000000000000000, -1.000000000000000000 ) ) ;
#10882 = ORIENTED_EDGE ( 'NONE', *, *, #3977, .T. ) ;
#10883 = DIRECTION ( 'NONE',  ( -1.000000000000000000, 0.000000000000000000, 0.000000000000000000 ) ) ;
#10884 = DIRECTION ( 'NONE',  ( -0.000000000000000000, -0.000000000000000000, 1.000000000000000000 ) ) ;
#10885 = ORIENTED_EDGE ( 'NONE', *, *, #1878, .T. ) ;
#10886 = ORIENTED_EDGE ( 'NONE', *, *, #2230, .F. ) ;
#10887 = VECTOR ( 'NONE', #9839, 1000.000000000000000 ) ;
#10888 = CARTESIAN_POINT ( 'NONE',  ( 307.5000000000000000, -36.99999999999997868, -169.9999999999999716 ) ) ;
#10889 = PRODUCT_DEFINITION_SHAPE ( 'NONE', 'NONE',  #14337 ) ;
#10890 = DIRECTION ( 'NONE',  ( 0.000000000000000000, -1.000000000000000000, 1.287488025362403787E-15 ) ) ;
#10891 = EDGE_LOOP ( 'NONE', ( #11266, #6435, #5899, #4009 ) ) ;
#10892 = CARTESIAN_POINT ( 'NONE',  ( -30.00000000000002842, -15.00000000000000000, 240.0000000000000284 ) ) ;
#10893 = CIRCLE ( 'NONE', #10187, 2.700000000000000622 ) ;
#10894 = FACE_OUTER_BOUND ( 'NONE', #7547, .T. ) ;
#10895 = CARTESIAN_POINT ( 'NONE',  ( -30.00000000000002842, -25.00000000000000000, 190.0000000000000000 ) ) ;
#10896 = CONTEXT_DEPENDENT_SHAPE_REPRESENTATION ( #12490, #9249 ) ;
#10897 = FACE_OUTER_BOUND ( 'NONE', #8656, .T. ) ;
#10898 = ORIENTED_EDGE ( 'NONE', *, *, #10780, .F. ) ;
#10899 = ORIENTED_EDGE ( 'NONE', *, *, #1262, .T. ) ;
#10900 = CARTESIAN_POINT ( 'NONE',  ( 134.9999999999999432, -56.99999999999997158, -180.0000000000000000 ) ) ;
#10901 = ORIENTED_EDGE ( 'NONE', *, *, #3658, .F. ) ;
#10902 = VECTOR ( 'NONE', #14128, 1000.000000000000000 ) ;
#10903 = DIRECTION ( 'NONE',  ( -1.000000000000000000, 0.000000000000000000, 0.000000000000000000 ) ) ;
#10904 = EDGE_LOOP ( 'NONE', ( #7694, #7142, #8812, #3579 ) ) ;
#10905 = ORIENTED_EDGE ( 'NONE', *, *, #11691, .T. ) ;
#10906 = PLANE ( 'NONE',  #7344 ) ;
#10907 = ORIENTED_EDGE ( 'NONE', *, *, #6735, .F. ) ;
#10908 = EDGE_CURVE ( 'NONE', #4652, #4058, #9505, .T. ) ;
#10909 = DIRECTION ( 'NONE',  ( -1.000000000000000000, 0.000000000000000000, 0.000000000000000000 ) ) ;
#10910 = CARTESIAN_POINT ( 'NONE',  ( 302.5000000000000000, -56.99999999999997158, -169.9999999999999716 ) ) ;
#10911 = DIRECTION ( 'NONE',  ( -0.000000000000000000, -0.000000000000000000, 1.000000000000000000 ) ) ;
#10912 = DIRECTION ( 'NONE',  ( -0.000000000000000000, -0.000000000000000000, -1.000000000000000000 ) ) ;
#10913 = AXIS2_PLACEMENT_3D ( 'NONE', #12744, #8169, #1420 ) ;
#10914 = LINE ( 'NONE', #7707, #5598 ) ;
#10915 = DIRECTION ( 'NONE',  ( 1.000000000000000000, 0.000000000000000000, 0.000000000000000000 ) ) ;
#10916 = ORIENTED_EDGE ( 'NONE', *, *, #10403, .F. ) ;
#10917 = AXIS2_PLACEMENT_3D ( 'NONE', #7928, #1939, #5554 ) ;
#10918 = EDGE_LOOP ( 'NONE', ( #1058, #4773, #1916, #2238, #9747 ) ) ;
#10919 = FACE_OUTER_BOUND ( 'NONE', #2222, .T. ) ;
#10920 = CIRCLE ( 'NONE', #13913, 5.560781378645573980 ) ;
#10921 = ORIENTED_EDGE ( 'NONE', *, *, #1602, .F. ) ;
#10922 = DIRECTION ( 'NONE',  ( 1.000000000000000000, 0.000000000000000000, 0.000000000000000000 ) ) ;
#10923 = ADVANCED_FACE ( 'NONE', ( #9433 ), #13772, .F. ) ;
#10924 = CARTESIAN_POINT ( 'NONE',  ( 2.740000000000000213, -0.6774776749089230776, 0.5149999999999995692 ) ) ;
#10925 = PRODUCT_DEFINITION ( 'UNKNOWN', '', #7247, #6366 ) ;
#10926 = DIRECTION ( 'NONE',  ( 1.000000000000000000, 0.000000000000000000, 0.000000000000000000 ) ) ;
#10927 = EDGE_LOOP ( 'NONE', ( #9796, #11629 ) ) ;
#10928 = AXIS2_PLACEMENT_3D ( 'NONE', #7561, #11859, #9611 ) ;
#10929 = CARTESIAN_POINT ( 'NONE',  ( 299.9999999999999432, -95.00000000000008527, 190.0000000000000000 ) ) ;
#10930 = DIRECTION ( 'NONE',  ( -0.000000000000000000, -0.000000000000000000, -1.000000000000000000 ) ) ;
#10931 = DIRECTION ( 'NONE',  ( -1.000000000000000000, 0.000000000000000000, 6.123233995736766036E-17 ) ) ;
#10932 = VECTOR ( 'NONE', #9551, 1000.000000000000000 ) ;
#10933 = CARTESIAN_POINT ( 'NONE',  ( -4.211140560182196957, -2.431303136016552013, -3.745885042887436178 ) ) ;
#10934 = EDGE_CURVE ( 'NONE', #6925, #11920, #12833, .T. ) ;
#10935 = EDGE_CURVE ( 'NONE', #8786, #14065, #6236, .T. ) ;
#10936 = EDGE_LOOP ( 'NONE', ( #8552, #12464 ) ) ;
#10937 = STYLED_ITEM ( 'NONE', ( #3911 ), #1248 ) ;
#10938 = EDGE_CURVE ( 'NONE', #5289, #8791, #6300, .T. ) ;
#10939 = ORIENTED_EDGE ( 'NONE', *, *, #2151, .F. ) ;
#10940 = CARTESIAN_POINT ( 'NONE',  ( 294.4999999999999432, -75.00000000000008527, 190.0000000000000000 ) ) ;
#10941 = DIRECTION ( 'NONE',  ( 1.000000000000000000, 0.000000000000000000, 0.000000000000000000 ) ) ;
#10942 = CONICAL_SURFACE ( 'NONE', #4686, 4.000000000000000000, 0.8911886515913786111 ) ;
#10944 = ORIENTED_EDGE ( 'NONE', *, *, #10403, .T. ) ;
#10943 = AXIS2_PLACEMENT_3D ( 'NONE', #2236, #2448, #3411 ) ;
#10945 = CARTESIAN_POINT ( 'NONE',  ( 3.999999999999999112, -0.3979232138631231819, -5.929230630780099908E-17 ) ) ;
#10946 = AXIS2_PLACEMENT_3D ( 'NONE', #10568, #7444, #6137 ) ;
#10947 =( LENGTH_UNIT ( ) NAMED_UNIT ( * ) SI_UNIT ( .MILLI., .METRE. ) );
#10948 = VECTOR ( 'NONE', #1005, 1000.000000000000000 ) ;
#10949 = CARTESIAN_POINT ( 'NONE',  ( 12.00000000000000000, 1.469576158976823947E-15, -186.0000000000000000 ) ) ;
#10950 = DIRECTION ( 'NONE',  ( -1.000000000000000000, 0.000000000000000000, 0.000000000000000000 ) ) ;
#10951 = CIRCLE ( 'NONE', #12558, 0.8509999999999999787 ) ;
#10952 = EDGE_CURVE ( 'NONE', #2298, #140, #12361, .T. ) ;
#10953 = ORIENTED_EDGE ( 'NONE', *, *, #9762, .T. ) ;
#10954 = CARTESIAN_POINT ( 'NONE',  ( 197.5000000000000000, -80.00000000000007105, 55.00000000000001421 ) ) ;
#10955 = VECTOR ( 'NONE', #9168, 1000.000000000000000 ) ;
#10956 = B_SPLINE_CURVE_WITH_KNOTS ( 'NONE', 3,
 ( #1255, #8143, #13662, #12583 ),
 .UNSPECIFIED., .F., .F.,
 ( 4, 4 ),
 ( 0.001586480563516617188, 0.004268227385920363680 ),
 .UNSPECIFIED. ) ;
#10957 = EDGE_LOOP ( 'NONE', ( #3634, #7710, #1841, #272, #6015 ) ) ;
#10958 = CARTESIAN_POINT ( 'NONE',  ( 0.000000000000000000, 0.000000000000000000, 11.75000000000000000 ) ) ;
#10959 = B_SPLINE_CURVE_WITH_KNOTS ( 'NONE', 3,
 ( #11831, #11611, #1954, #11761 ),
 .UNSPECIFIED., .F., .F.,
 ( 4, 4 ),
 ( 0.000000000000000000, 0.002452478801916376308 ),
 .UNSPECIFIED. ) ;
#10960 = EDGE_CURVE ( 'NONE', #924, #1149, #1985, .T. ) ;
#10961 =( REPRESENTATION_RELATIONSHIP ('NONE','NONE', #11251, #2275 ) REPRESENTATION_RELATIONSHIP_WITH_TRANSFORMATION ( #1800 )SHAPE_REPRESENTATION_RELATIONSHIP( ) );
#10962 = EDGE_LOOP ( 'NONE', ( #3761, #4380 ) ) ;
#10963 = VERTEX_POINT ( 'NONE', #14269 ) ;
#10964 = DIRECTION ( 'NONE',  ( -0.000000000000000000, 1.000000000000000000, 0.000000000000000000 ) ) ;
#10965 = FACE_OUTER_BOUND ( 'NONE', #7319, .T. ) ;
#10967 = VERTEX_POINT ( 'NONE', #842 ) ;
#10966 = AXIS2_PLACEMENT_3D ( 'NONE', #11067, #8738, #12142 ) ;
#10968 = DIRECTION ( 'NONE',  ( 1.000000000000000000, 0.000000000000000000, 0.000000000000000000 ) ) ;
#10969 = PLANE ( 'NONE',  #6057 ) ;
#10970 = CARTESIAN_POINT ( 'NONE',  ( 386.6666666666666288, -20.00000000000000000, 222.5000000000000853 ) ) ;
#10971 = PLANE ( 'NONE',  #11267 ) ;
#10972 = PRESENTATION_STYLE_ASSIGNMENT (( #11174 ) ) ;
#10973 = CARTESIAN_POINT ( 'NONE',  ( 82.99999999999998579, 8.660254037844390851, 200.0000000000000000 ) ) ;
#10974 = CARTESIAN_POINT ( 'NONE',  ( -4.000000000000000000, -2.512220745329312610, -3.469390707569719901 ) ) ;
#10975 = ORIENTED_EDGE ( 'NONE', *, *, #12842, .T. ) ;
#10976 = ORIENTED_EDGE ( 'NONE', *, *, #13401, .T. ) ;
#10977 = DIRECTION ( 'NONE',  ( 0.000000000000000000, 1.000000000000000000, 0.000000000000000000 ) ) ;
#10978 = ORIENTED_EDGE ( 'NONE', *, *, #9349, .T. ) ;
#10979 = LINE ( 'NONE', #13139, #9326 ) ;
#10980 = ORIENTED_EDGE ( 'NONE', *, *, #4544, .T. ) ;
#10981 = ORIENTED_EDGE ( 'NONE', *, *, #10083, .T. ) ;
#10982 = CARTESIAN_POINT ( 'NONE',  ( -299.9999999999999432, -75.00000000000008527, 354.1421356237308942 ) ) ;
#10983 = ORIENTED_EDGE ( 'NONE', *, *, #11547, .T. ) ;
#10984 = CARTESIAN_POINT ( 'NONE',  ( -140.0000000000000000, -95.00000000000008527, 40.00000000000000000 ) ) ;
#10985 = CARTESIAN_POINT ( 'NONE',  ( 53.33333333333330017, -20.00000000000000000, -219.8500000000001080 ) ) ;
#10986 = CARTESIAN_POINT ( 'NONE',  ( 236.4999999999999432, -85.00000000000007105, 180.0000000000000000 ) ) ;
#10987 = EDGE_CURVE ( 'NONE', #10282, #8744, #6095, .T. ) ;
#10988 = CARTESIAN_POINT ( 'NONE',  ( 2.500000000000000000, 2.357898499370433054, -1.951563910473907981E-15 ) ) ;
#10989 = PLANE ( 'NONE',  #9975 ) ;
#10990 = DIRECTION ( 'NONE',  ( -1.000000000000000000, -0.000000000000000000, -0.000000000000000000 ) ) ;
#10991 = VERTEX_POINT ( 'NONE', #12983 ) ;
#10992 = ORIENTED_EDGE ( 'NONE', *, *, #3677, .F. ) ;
#10993 = DIRECTION ( 'NONE',  ( -0.000000000000000000, -0.000000000000000000, -1.000000000000000000 ) ) ;
#10994 = ORIENTED_EDGE ( 'NONE', *, *, #2878, .F. ) ;
#10995 = CARTESIAN_POINT ( 'NONE',  ( 140.0000000000000000, -95.00000000000008527, -190.0000000000000000 ) ) ;
#10996 = LINE ( 'NONE', #10783, #1191 ) ;
#10997 = FACE_OUTER_BOUND ( 'NONE', #12048, .T. ) ;
#10998 = ORIENTED_EDGE ( 'NONE', *, *, #9552, .T. ) ;
#10999 = CARTESIAN_POINT ( 'NONE',  ( 137.6499999999999488, -56.99999999999997158, 10.00000000000000000 ) ) ;
#11000 = CARTESIAN_POINT ( 'NONE',  ( 305.0000000000000000, -56.99999999999997158, -181.5021515430661054 ) ) ;
#11001 = CARTESIAN_POINT ( 'NONE',  ( 136.6666666666666288, -20.00000000000000000, 222.5000000000000853 ) ) ;
#11002 = EDGE_CURVE ( 'NONE', #1558, #9645, #7934, .T. ) ;
#11003 = ORIENTED_EDGE ( 'NONE', *, *, #10861, .T. ) ;
#11004 = ADVANCED_FACE ( 'NONE', ( #7466 ), #12907, .F. ) ;
#11005 = CARTESIAN_POINT ( 'NONE',  ( 5.200000000000002842, 0.000000000000000000, 0.000000000000000000 ) ) ;
#11006 = PRODUCT_DEFINITION_SHAPE ( 'NONE', 'NONE',  #14338 ) ;
#11007 = AXIS2_PLACEMENT_3D ( 'NONE', #9377, #6332, #3000 ) ;
#11008 = DIRECTION ( 'NONE',  ( 0.000000000000000000, -0.4999999999999989453, 0.8660254037844391517 ) ) ;
#11009 = ORIENTED_EDGE ( 'NONE', *, *, #10325, .F. ) ;
#11010 = CARTESIAN_POINT ( 'NONE',  ( 4.000000000000000000, 0.000000000000000000, 0.000000000000000000 ) ) ;
#11011 = EDGE_CURVE ( 'NONE', #1125, #10453, #6454, .T. ) ;
#11012 = PLANE ( 'NONE',  #3185 ) ;
#11013 = DIRECTION ( 'NONE',  ( 0.000000000000000000, 0.000000000000000000, 1.000000000000000000 ) ) ;
#11014 = DIRECTION ( 'NONE',  ( 0.000000000000000000, 0.000000000000000000, 1.000000000000000000 ) ) ;
#11015 = AXIS2_PLACEMENT_3D ( 'NONE', #7832, #12476, #6819 ) ;
#11016 =( REPRESENTATION_RELATIONSHIP ('NONE','NONE', #11251, #9307 ) REPRESENTATION_RELATIONSHIP_WITH_TRANSFORMATION ( #5240 )SHAPE_REPRESENTATION_RELATIONSHIP( ) );
#11017 = ADVANCED_FACE ( 'NONE', ( #4351 ), #3528, .F. ) ;
#11018 = CONTEXT_DEPENDENT_SHAPE_REPRESENTATION ( #5485, #1953 ) ;
#11019 = ORIENTED_EDGE ( 'NONE', *, *, #531, .T. ) ;
#11020 = LINE ( 'NONE', #6451, #6847 ) ;
#11021 = EDGE_LOOP ( 'NONE', ( #9313, #11203, #7412, #9289, #9442 ) ) ;
#11022 = DIRECTION ( 'NONE',  ( -0.000000000000000000, 0.000000000000000000, -1.000000000000000000 ) ) ;
#11023 = DIRECTION ( 'NONE',  ( -0.000000000000000000, -0.000000000000000000, -1.000000000000000000 ) ) ;
#11024 = CIRCLE ( 'NONE', #12870, 4.250000000000000000 ) ;
#11025 = ORIENTED_EDGE ( 'NONE', *, *, #2163, .F. ) ;
#11026 = ORIENTED_EDGE ( 'NONE', *, *, #9596, .F. ) ;
#11027 = PLANE ( 'NONE',  #13111 ) ;
#11028 = EDGE_CURVE ( 'NONE', #9436, #5881, #219, .T. ) ;
#11029 = EDGE_CURVE ( 'NONE', #5322, #3720, #7601, .T. ) ;
#11030 = UNCERTAINTY_MEASURE_WITH_UNIT (LENGTH_MEASURE( 1.000000000000000082E-05 ), #8033, 'distance_accuracy_value', 'NONE');
#11031 = DIRECTION ( 'NONE',  ( 0.000000000000000000, 0.8660254037844380415, -0.5000000000000012212 ) ) ;
#11032 =( NAMED_UNIT ( * ) PLANE_ANGLE_UNIT ( ) SI_UNIT ( $, .RADIAN. ) );
#11033 = EDGE_CURVE ( 'NONE', #3920, #8960, #8349, .T. ) ;
#11034 = EDGE_CURVE ( 'NONE', #5038, #9120, #768, .T. ) ;
#11035 = CARTESIAN_POINT ( 'NONE',  ( -30.00000000000002842, -225.0000000000000000, -169.9999999999999716 ) ) ;
#11036 = CARTESIAN_POINT ( 'NONE',  ( 5.560781378645573980, 6.809993116116507654E-16, -4.000000000000000000 ) ) ;
#11037 = DIRECTION ( 'NONE',  ( -0.000000000000000000, -0.000000000000000000, -1.000000000000000000 ) ) ;
#11038 = CARTESIAN_POINT ( 'NONE',  ( 124.9999999999999858, 55.00000000000000711, 0.000000000000000000 ) ) ;
#11039 = EDGE_CURVE ( 'NONE', #2887, #12966, #1649, .T. ) ;
#11040 = DIRECTION ( 'NONE',  ( 0.000000000000000000, 1.000000000000000000, 0.000000000000000000 ) ) ;
#11041 = AXIS2_PLACEMENT_3D ( 'NONE', #4948, #12769, #9367 ) ;
#11042 = ORIENTED_EDGE ( 'NONE', *, *, #11218, .T. ) ;
#11043 = EDGE_LOOP ( 'NONE', ( #7960, #4653, #10371, #1942 ) ) ;
#11044 = CIRCLE ( 'NONE', #8518, 2.649999999999985700 ) ;
#11045 = CARTESIAN_POINT ( 'NONE',  ( -304.9999999999999432, -75.00000000000008527, 339.9999999999999432 ) ) ;
#11046 = VERTEX_POINT ( 'NONE', #1876 ) ;
#11047 = PLANE ( 'NONE',  #10485 ) ;
#11048 = ORIENTED_EDGE ( 'NONE', *, *, #5991, .F. ) ;
#11049 = CARTESIAN_POINT ( 'NONE',  ( 21.00000000000000355, 0.000000000000000000, 2.055000000000000160 ) ) ;
#11050 = ORIENTED_EDGE ( 'NONE', *, *, #2658, .F. ) ;
#11052 = DIRECTION ( 'NONE',  ( -1.000000000000000000, 0.000000000000000000, 0.000000000000000000 ) ) ;
#11051 = AXIS2_PLACEMENT_3D ( 'NONE', #8908, #27, #7869 ) ;
#11053 = CIRCLE ( 'NONE', #10576, 4.250000000000000000 ) ;
#11054 = DIRECTION ( 'NONE',  ( 0.000000000000000000, 0.000000000000000000, 1.000000000000000000 ) ) ;
#11055 = DIRECTION ( 'NONE',  ( -0.000000000000000000, 1.000000000000000000, -0.000000000000000000 ) ) ;
#11056 = CIRCLE ( 'NONE', #8009, 5.500000000000005329 ) ;
#11057 = DIRECTION ( 'NONE',  ( 0.000000000000000000, 0.8660254037844380415, -0.5000000000000012212 ) ) ;
#11058 = SURFACE_SIDE_STYLE ('',( #7910 ) ) ;
#11059 = FILL_AREA_STYLE ('',( #1016 ) ) ;
#11060 = DIRECTION ( 'NONE',  ( 0.000000000000000000, -0.000000000000000000, 1.000000000000000000 ) ) ;
#11061 = VECTOR ( 'NONE', #11595, 1000.000000000000000 ) ;
#11062 = ORIENTED_EDGE ( 'NONE', *, *, #5467, .F. ) ;
#11063 = EDGE_LOOP ( 'NONE', ( #10245, #3561, #8327, #6704 ) ) ;
#11064 = VECTOR ( 'NONE', #13077, 1000.000000000000114 ) ;
#11065 = EDGE_CURVE ( 'NONE', #3716, #8006, #5370, .T. ) ;
#11067 = CARTESIAN_POINT ( 'NONE',  ( 5.200000000000002842, 0.000000000000000000, -2.700000000000001066 ) ) ;
#11066 = AXIS2_PLACEMENT_3D ( 'NONE', #3633, #4660, #7969 ) ;
#11068 = AXIS2_PLACEMENT_3D ( 'NONE', #11470, #11331, #7972 ) ;
#11069 = VERTEX_POINT ( 'NONE', #12039 ) ;
#11070 = CARTESIAN_POINT ( 'NONE',  ( 470.0000000000000000, 15.00000000000000000, 200.0000000000000000 ) ) ;
#11071 = DIRECTION ( 'NONE',  ( 0.000000000000000000, 0.000000000000000000, 1.000000000000000000 ) ) ;
#11072 = DIRECTION ( 'NONE',  ( 0.4461977533473793778, 0.8949343913984707521, -1.884057886186824495E-16 ) ) ;
#11073 = AXIS2_PLACEMENT_3D ( 'NONE', #14096, #4166, #7563 ) ;
#11074 = ORIENTED_EDGE ( 'NONE', *, *, #3752, .F. ) ;
#11075 = AXIS2_PLACEMENT_3D ( 'NONE', #13200, #993, #14072 ) ;
#11076 = CARTESIAN_POINT ( 'NONE',  ( 145.5000000000000284, -75.00000000000008527, 186.2999999999999829 ) ) ;
#11077 = CARTESIAN_POINT ( 'NONE',  ( 357.0000000000000000, 8.660254037844390851, 205.0000000000000284 ) ) ;
#11078 = VECTOR ( 'NONE', #7901, 1000.000000000000000 ) ;
#11079 = DIRECTION ( 'NONE',  ( -0.000000000000000000, 0.000000000000000000, 1.000000000000000000 ) ) ;
#11080 = CIRCLE ( 'NONE', #11730, 2.041999999999999815 ) ;
#11081 = DIRECTION ( 'NONE',  ( 0.000000000000000000, 0.000000000000000000, 1.000000000000000000 ) ) ;
#11082 = EDGE_LOOP ( 'NONE', ( #1692, #6608, #1949, #964 ) ) ;
#11083 = EDGE_CURVE ( 'NONE', #11920, #6551, #13018, .T. ) ;
#11084 = DIRECTION ( 'NONE',  ( 0.000000000000000000, 0.000000000000000000, -1.000000000000000000 ) ) ;
#11085 = PRESENTATION_LAYER_ASSIGNMENT (  '', '', ( #5478 ) ) ;
#11086 = CARTESIAN_POINT ( 'NONE',  ( 136.6666666666666288, -20.00000000000000000, 219.8500000000001080 ) ) ;
#11087 = CARTESIAN_POINT ( 'NONE',  ( -135.0000000000000000, -95.00000000000008527, 40.00000000000000000 ) ) ;
#11088 = EDGE_LOOP ( 'NONE', ( #13775, #13870, #3928, #12611 ) ) ;
#11090 = EDGE_CURVE ( 'NONE', #634, #11403, #11899, .T. ) ;
#11089 = DIRECTION ( 'NONE',  ( 1.000000000000000000, 0.000000000000000000, 0.000000000000000000 ) ) ;
#11091 = DIRECTION ( 'NONE',  ( 1.000000000000000000, 0.000000000000000000, 0.000000000000000000 ) ) ;
#11092 = DIRECTION ( 'NONE',  ( -0.000000000000000000, -0.000000000000000000, -1.000000000000000000 ) ) ;
#11093 = CARTESIAN_POINT ( 'NONE',  ( 88.00000000000000000, 0.000000000000000000, 0.000000000000000000 ) ) ;
#11094 = CIRCLE ( 'NONE', #6689, 2.649999999999985700 ) ;
#11095 = EDGE_LOOP ( 'NONE', ( #8692, #14227, #2451 ) ) ;
#11096 = DIRECTION ( 'NONE',  ( -0.000000000000000000, -0.000000000000000000, 1.000000000000000000 ) ) ;
#11097 = PRODUCT_DEFINITION_SHAPE ( 'NONE', 'NONE',  #6833 ) ;
#11098 = ORIENTED_EDGE ( 'NONE', *, *, #4097, .T. ) ;
#11099 = CARTESIAN_POINT ( 'NONE',  ( -4.000000000000000000, -0.7890432684750890990, -0.04868663549882315533 ) ) ;
#11100 = ORIENTED_EDGE ( 'NONE', *, *, #13401, .F. ) ;
#11101 = EDGE_LOOP ( 'NONE', ( #1605, #7051, #1048, #12387 ) ) ;
#11103 = ADVANCED_FACE ( 'NONE', ( #8628 ), #3126, .T. ) ;
#11102 = DIRECTION ( 'NONE',  ( -1.000000000000000000, 0.000000000000000000, 0.000000000000000000 ) ) ;
#11104 = EDGE_CURVE ( 'NONE', #3478, #4659, #9797, .T. ) ;
#11105 = DIRECTION ( 'NONE',  ( -0.000000000000000000, -0.000000000000000000, 1.000000000000000000 ) ) ;
#11106 = APPLICATION_CONTEXT ( 'automotive_design' ) ;
#11107 = DIRECTION ( 'NONE',  ( 0.000000000000000000, 0.000000000000000000, 1.000000000000000000 ) ) ;
#11108 = AXIS2_PLACEMENT_3D ( 'NONE', #3424, #5588, #7826 ) ;
#11109 = CARTESIAN_POINT ( 'NONE',  ( 2.500000000000000000, 2.357898499370433054, -1.951563910473907981E-15 ) ) ;
#11110 = CARTESIAN_POINT ( 'NONE',  ( -0.6666666666666666297, -4.233901974057276973, -3.300726591567087365 ) ) ;
#11111 = CARTESIAN_POINT ( 'NONE',  ( -2.000000000000001776, 0.000000000000000000, -12.77500000000000036 ) ) ;
#11112 = DIRECTION ( 'NONE',  ( -0.000000000000000000, 1.000000000000000000, -0.000000000000000000 ) ) ;
#11113 = VERTEX_POINT ( 'NONE', #8695 ) ;
#11114 = VERTEX_POINT ( 'NONE', #3201 ) ;
#11115 = ADVANCED_FACE ( 'NONE', ( #2094 ), #7174, .F. ) ;
#11116 = EDGE_CURVE ( 'NONE', #11674, #498, #9079, .T. ) ;
#11117 = LINE ( 'NONE', #10026, #8211 ) ;
#11118 = ORIENTED_EDGE ( 'NONE', *, *, #4827, .F. ) ;
#11119 = EDGE_CURVE ( 'NONE', #3734, #2838, #3609, .T. ) ;
#11120 = LINE ( 'NONE', #14151, #7001 ) ;
#11121 = VECTOR ( 'NONE', #13184, 1000.000000000000000 ) ;
#11122 = VERTEX_POINT ( 'NONE', #8019 ) ;
#11123 = CARTESIAN_POINT ( 'NONE',  ( -134.9999999999999716, 45.00000000000001421, 30.00000000000000000 ) ) ;
#11124 = ORIENTED_EDGE ( 'NONE', *, *, #9314, .F. ) ;
#11125 = DIRECTION ( 'NONE',  ( 0.000000000000000000, 0.000000000000000000, -1.000000000000000000 ) ) ;
#11126 = CARTESIAN_POINT ( 'NONE',  ( 4.000000000000000000, 2.309401076758497151, -3.433295621305379353 ) ) ;
#11127 = B_SPLINE_CURVE_WITH_KNOTS ( 'NONE', 3,
 ( #5938, #10290, #6011, #12472, #9063, #9132 ),
 .UNSPECIFIED., .F., .F.,
 ( 4, 2, 4 ),
 ( 0.002365888236227995517, 0.003551327329835084114, 0.004736766423442172712 ),
 .UNSPECIFIED. ) ;
#11128 = DIRECTION ( 'NONE',  ( 1.000000000000000000, 0.000000000000000000, 0.000000000000000000 ) ) ;
#11129 = DIRECTION ( 'NONE',  ( -1.000000000000000000, 0.000000000000000000, 0.000000000000000000 ) ) ;
#11130 = AXIS2_PLACEMENT_3D ( 'NONE', #1776, #816, #9702 ) ;
#11131 = DIRECTION ( 'NONE',  ( 0.000000000000000000, 0.000000000000000000, -1.000000000000000000 ) ) ;
#11132 = ORIENTED_EDGE ( 'NONE', *, *, #4469, .F. ) ;
#11133 = VECTOR ( 'NONE', #698, 1000.000000000000000 ) ;
#11134 = EDGE_LOOP ( 'NONE', ( #12835, #7758, #1875, #4965 ) ) ;
#11135 = AXIS2_PLACEMENT_3D ( 'NONE', #2700, #7119, #13640 ) ;
#11136 = CARTESIAN_POINT ( 'NONE',  ( 21.00000000000000000, 2.055000000000000160, 0.000000000000000000 ) ) ;
#11137 = ORIENTED_EDGE ( 'NONE', *, *, #13056, .T. ) ;
#11138 = CARTESIAN_POINT ( 'NONE',  ( -299.9999999999999432, -75.00000000000008527, 30.00000000000002842 ) ) ;
#11139 = CARTESIAN_POINT ( 'NONE',  ( 136.6666666666666288, -15.00000000000000000, 222.5000000000000853 ) ) ;
#11140 = AXIS2_PLACEMENT_3D ( 'NONE', #10795, #5145, #1933 ) ;
#11141 = DIRECTION ( 'NONE',  ( -0.000000000000000000, -0.000000000000000000, -1.000000000000000000 ) ) ;
#11142 = EDGE_CURVE ( 'NONE', #2517, #2327, #12462, .T. ) ;
#11143 = CARTESIAN_POINT ( 'NONE',  ( 21.00000000000000355, 0.000000000000000000, 0.000000000000000000 ) ) ;
#11144 = DIRECTION ( 'NONE',  ( 1.000000000000000000, 0.000000000000000000, 0.000000000000000000 ) ) ;
#11145 = CARTESIAN_POINT ( 'NONE',  ( 124.9999999999999574, -64.99999999999997158, 10.00000000000000000 ) ) ;
#11146 = ORIENTED_EDGE ( 'NONE', *, *, #1089, .F. ) ;
#11147 = VECTOR ( 'NONE', #970, 1000.000000000000000 ) ;
#11148 = AXIS2_PLACEMENT_3D ( 'NONE', #10053, #3802, #6919 ) ;
#11149 = CARTESIAN_POINT ( 'NONE',  ( 28.70000000000000284, 3.061616997868383141E-16, -2.500000000000000000 ) ) ;
#11150 = DIRECTION ( 'NONE',  ( 0.000000000000000000, 0.000000000000000000, 1.000000000000000000 ) ) ;
#11151 = DIRECTION ( 'NONE',  ( 0.000000000000000000, 1.224646799147361589E-16, 1.000000000000000000 ) ) ;
#11152 = EDGE_LOOP ( 'NONE', ( #6092, #8937, #11950, #4394 ) ) ;
#11153 = DIRECTION ( 'NONE',  ( 0.8660254037844379305, 0.5000000000000013323, 0.000000000000000000 ) ) ;
#11154 = VECTOR ( 'NONE', #9401, 1000.000000000000000 ) ;
#11155 = DIRECTION ( 'NONE',  ( 0.000000000000000000, 0.000000000000000000, 1.000000000000000000 ) ) ;
#11156 = EDGE_CURVE ( 'NONE', #2710, #4356, #946, .T. ) ;
#11157 = CARTESIAN_POINT ( 'NONE',  ( -124.9999999999999432, 55.00000000000001421, 30.00000000000000000 ) ) ;
#11158 = DIRECTION ( 'NONE',  ( 1.000000000000000000, 0.000000000000000000, 0.000000000000000000 ) ) ;
#11159 = CONTEXT_DEPENDENT_SHAPE_REPRESENTATION ( #4553, #11566 ) ;
#11160 = ORIENTED_EDGE ( 'NONE', *, *, #1897, .T. ) ;
#11161 = ADVANCED_FACE ( 'NONE', ( #6870 ), #5505, .T. ) ;
#11162 = CARTESIAN_POINT ( 'NONE',  ( 24.55500000000002103, 0.000000000000000000, 0.000000000000000000 ) ) ;
#11163 = AXIS2_PLACEMENT_3D ( 'NONE', #12721, #2790, #7205 ) ;
#11164 = ORIENTED_EDGE ( 'NONE', *, *, #4492, .T. ) ;
#11165 = CARTESIAN_POINT ( 'NONE',  ( -124.9999999999999432, -105.0000000000000853, 30.00000000000000000 ) ) ;
#11166 = ORIENTED_EDGE ( 'NONE', *, *, #8678, .F. ) ;
#11167 = EDGE_LOOP ( 'NONE', ( #6527, #7929, #9271, #9364 ) ) ;
#11168 = DIRECTION ( 'NONE',  ( -1.000000000000000000, -0.000000000000000000, -0.000000000000000000 ) ) ;
#11169 = CARTESIAN_POINT ( 'NONE',  ( -299.9999999999999432, -75.00000000000008527, 329.9999999999999432 ) ) ;
#11170 = CARTESIAN_POINT ( 'NONE',  ( -219.9999999999999147, -85.00000000000009948, 40.00000000000000000 ) ) ;
#11171 = FACE_BOUND ( 'NONE', #12008, .T. ) ;
#11172 = DIRECTION ( 'NONE',  ( 0.000000000000000000, 0.000000000000000000, 1.000000000000000000 ) ) ;
#11173 = CARTESIAN_POINT ( 'NONE',  ( 242.5000000000000000, -90.00000000000007105, 55.00000000000001421 ) ) ;
#11174 = SURFACE_STYLE_USAGE ( .BOTH. , #12261 ) ;
#11175 = VECTOR ( 'NONE', #621, 1000.000000000000000 ) ;
#11176 = DIRECTION ( 'NONE',  ( -1.000000000000000000, 0.000000000000000000, 0.000000000000000000 ) ) ;
#11177 = CONTEXT_DEPENDENT_SHAPE_REPRESENTATION ( #7706, #11683 ) ;
#11178 = CARTESIAN_POINT ( 'NONE',  ( 0.000000000000000000, 8.660254037844390851, 200.0000000000000000 ) ) ;
#11179 = AXIS2_PLACEMENT_3D ( 'NONE', #3895, #9478, #4039 ) ;
#11180 = ORIENTED_EDGE ( 'NONE', *, *, #3862, .T. ) ;
#11181 = CIRCLE ( 'NONE', #4691, 2.100000000000000089 ) ;
#11182 = EDGE_LOOP ( 'NONE', ( #1523, #8201 ) ) ;
#11183 = EDGE_CURVE ( 'NONE', #2006, #4356, #13558, .T. ) ;
#11184 = CARTESIAN_POINT ( 'NONE',  ( 0.3226060873438262311, 0.5150000000000077849, -2.189154565102684025 ) ) ;
#11185 = EDGE_CURVE ( 'NONE', #3774, #3034, #14129, .T. ) ;
#11186 = ORIENTED_EDGE ( 'NONE', *, *, #11905, .T. ) ;
#11187 = CARTESIAN_POINT ( 'NONE',  ( 0.000000000000000000, 1.178949249685213863, -2.042000000000001148 ) ) ;
#11188 = CIRCLE ( 'NONE', #13035, 2.649999999999985700 ) ;
#11189 = VERTEX_POINT ( 'NONE', #12385 ) ;
#11190 = DIRECTION ( 'NONE',  ( 0.000000000000000000, 0.000000000000000000, -1.000000000000000000 ) ) ;
#11191 = ORIENTED_EDGE ( 'NONE', *, *, #6565, .T. ) ;
#11192 = DIRECTION ( 'NONE',  ( 1.000000000000000000, 0.000000000000000000, 0.000000000000000000 ) ) ;
#11193 = AXIS2_PLACEMENT_3D ( 'NONE', #10769, #13872, #11998 ) ;
#11194 = DIRECTION ( 'NONE',  ( -0.000000000000000000, -0.000000000000000000, 1.000000000000000000 ) ) ;
#11195 = SURFACE_SIDE_STYLE ('',( #13291 ) ) ;
#11196 = EDGE_CURVE ( 'NONE', #865, #9564, #13327, .T. ) ;
#11197 = CARTESIAN_POINT ( 'NONE',  ( 0.000000000000000000, 0.000000000000000000, 0.000000000000000000 ) ) ;
#11198 =( LENGTH_UNIT ( ) NAMED_UNIT ( * ) SI_UNIT ( .MILLI., .METRE. ) );
#11199 = DIRECTION ( 'NONE',  ( -1.000000000000000000, -0.000000000000000000, -0.000000000000000000 ) ) ;
#11200 = CARTESIAN_POINT ( 'NONE',  ( 305.0000000000000000, -56.99999999999997158, -154.9999999999999716 ) ) ;
#11201 = DIRECTION ( 'NONE',  ( 0.000000000000000000, 0.000000000000000000, -1.000000000000000000 ) ) ;
#11202 = AXIS2_PLACEMENT_3D ( 'NONE', #2756, #549, #9290 ) ;
#11203 = ORIENTED_EDGE ( 'NONE', *, *, #5848, .F. ) ;
#11204 = EDGE_CURVE ( 'NONE', #12064, #8653, #7744, .T. ) ;
#11205 = ORIENTED_EDGE ( 'NONE', *, *, #3986, .F. ) ;
#11206 = VERTEX_POINT ( 'NONE', #2384 ) ;
#11207 = DIRECTION ( 'NONE',  ( 0.000000000000000000, 0.000000000000000000, 1.000000000000000000 ) ) ;
#11208 = ORIENTED_EDGE ( 'NONE', *, *, #12447, .F. ) ;
#11209 = DIRECTION ( 'NONE',  ( -0.000000000000000000, 1.287488025362403787E-15, 1.000000000000000000 ) ) ;
#11210 = DIRECTION ( 'NONE',  ( 0.000000000000000000, 0.000000000000000000, -1.000000000000000000 ) ) ;
#11211 = CARTESIAN_POINT ( 'NONE',  ( 197.5000000000000000, -80.00000000000007105, 55.00000000000001421 ) ) ;
#11212 = EDGE_CURVE ( 'NONE', #9222, #8111, #2828, .T. ) ;
#11213 = DIRECTION ( 'NONE',  ( 1.000000000000000000, 0.000000000000000000, 0.000000000000000000 ) ) ;
#11214 = ADVANCED_FACE ( 'NONE', ( #7811 ), #4655, .F. ) ;
#11215 = DIRECTION ( 'NONE',  ( -0.000000000000000000, 1.000000000000000000, -0.000000000000000000 ) ) ;
#11216 = CARTESIAN_POINT ( 'NONE',  ( 2.000000000000001776, 1.641026710857453312E-15, 13.29999999999999893 ) ) ;
#11217 = CARTESIAN_POINT ( 'NONE',  ( 140.0000000000000000, -75.00000000000008527, 190.0000000000000000 ) ) ;
#11218 = EDGE_CURVE ( 'NONE', #6471, #8017, #6734, .T. ) ;
#11219 = VERTEX_POINT ( 'NONE', #99 ) ;
#11220 = DIRECTION ( 'NONE',  ( 0.8571673013836870192, 0.000000000000000000, 0.5150380737757234151 ) ) ;
#11221 = DIRECTION ( 'NONE',  ( 0.000000000000000000, 0.000000000000000000, 1.000000000000000000 ) ) ;
#11222 = DIRECTION ( 'NONE',  ( -1.000000000000000000, 0.000000000000000000, 0.000000000000000000 ) ) ;
#11223 = VERTEX_POINT ( 'NONE', #4562 ) ;
#11224 = DIRECTION ( 'NONE',  ( 1.000000000000000000, 0.000000000000000000, 0.000000000000000000 ) ) ;
#11225 = CYLINDRICAL_SURFACE ( 'NONE', #13876, 5.500000000000005329 ) ;
#11226 = DIRECTION ( 'NONE',  ( 6.123233995736766036E-17, -1.000000000000000000, 0.000000000000000000 ) ) ;
#11227 =( REPRESENTATION_RELATIONSHIP ('NONE','NONE', #11251, #11637 ) REPRESENTATION_RELATIONSHIP_WITH_TRANSFORMATION ( #7032 )SHAPE_REPRESENTATION_RELATIONSHIP( ) );
#11228 = VECTOR ( 'NONE', #2186, 1000.000000000000000 ) ;
#11229 = ORIENTED_EDGE ( 'NONE', *, *, #13389, .T. ) ;
#11230 = CARTESIAN_POINT ( 'NONE',  ( -1.799999999999996048, 1.249139735130300365E-15, 10.20000000000000107 ) ) ;
#11231 = EDGE_LOOP ( 'NONE', ( #8999, #7978 ) ) ;
#11232 = ADVANCED_FACE ( 'NONE', ( #8982 ), #5711, .F. ) ;
#11233 = CARTESIAN_POINT ( 'NONE',  ( -4.000000000000000000, -0.3979232138631226823, -3.896351557369779711E-17 ) ) ;
#11234 = ORIENTED_EDGE ( 'NONE', *, *, #9525, .T. ) ;
#11235 = EDGE_LOOP ( 'NONE', ( #4799, #2463, #10905 ) ) ;
#11236 = DIRECTION ( 'NONE',  ( -0.000000000000000000, -0.000000000000000000, -1.000000000000000000 ) ) ;
#11237 = LINE ( 'NONE', #387, #1787 ) ;
#11238 = CIRCLE ( 'NONE', #14014, 2.649999999999985700 ) ;
#11239 = CARTESIAN_POINT ( 'NONE',  ( 219.9999999999999716, -85.00000000000007105, 50.00000000000001421 ) ) ;
#11240 = CYLINDRICAL_SURFACE ( 'NONE', #7430, 2.100000000000000089 ) ;
#11241 = DIRECTION ( 'NONE',  ( -0.000000000000000000, -0.000000000000000000, -1.000000000000000000 ) ) ;
#11242 = CARTESIAN_POINT ( 'NONE',  ( 219.9999999999999147, -85.00000000000009948, -17.55500000000000327 ) ) ;
#11243 =( NAMED_UNIT ( * ) SI_UNIT ( $, .STERADIAN. ) SOLID_ANGLE_UNIT ( ) );
#11244 = CARTESIAN_POINT ( 'NONE',  ( 304.9999999999999432, 45.00000000000001421, 0.000000000000000000 ) ) ;
#11245 = ORIENTED_EDGE ( 'NONE', *, *, #12352, .T. ) ;
#11246 = ORIENTED_EDGE ( 'NONE', *, *, #8161, .T. ) ;
#11247 = FACE_OUTER_BOUND ( 'NONE', #12302, .T. ) ;
#11248 = ADVANCED_FACE ( 'NONE', ( #9270 ), #6036, .T. ) ;
#11249 = ORIENTED_EDGE ( 'NONE', *, *, #2089, .T. ) ;
#11250 = DIRECTION ( 'NONE',  ( 0.000000000000000000, -0.5000000000000013323, -0.8660254037844380415 ) ) ;
#11251 = SHAPE_REPRESENTATION ( 'MAS-197', ( #13497, #10007, #3746, #11866, #5610, #3072, #8615, #4681, #2367, #10472, #7909, #9784, #3530, #11634, #5372, #3311, #729, #11406, #13945, #9082, #7687, #12780, #7223, #1421, #5159, #1666, #13255, #10719, #9553, #6999, #2373, #8858, #4463, #12331, #13481, #5620, #2831, #2599, #3085, #9794, #12563, #6777, #489, #6304, #8147, #25, #1908, #13712, #10022, #3760, #7462, #10946, #11873, #5840, #1196, #3535, #10483, #7919, #9325, #8624, #11179, #4239, #2136, #11645, #4690, #4924, #13027, #6077, #5397, #7234, #14176, #13465, #949, #12794, #245, #6541, #8380 ), #256 ) ;
#11252 = ORIENTED_EDGE ( 'NONE', *, *, #1162, .T. ) ;
#11253 = DIRECTION ( 'NONE',  ( 0.000000000000000000, -2.105246936865057790E-16, 1.000000000000000000 ) ) ;
#11254 = ORIENTED_EDGE ( 'NONE', *, *, #10671, .T. ) ;
#11255 = CARTESIAN_POINT ( 'NONE',  ( 470.0000000000000000, -25.00000000000000000, -250.0000000000000000 ) ) ;
#11256 = CYLINDRICAL_SURFACE ( 'NONE', #7585, 2.500000000000002220 ) ;
#11257 = DIRECTION ( 'NONE',  ( 0.000000000000000000, 0.000000000000000000, 1.000000000000000000 ) ) ;
#11258 = EDGE_CURVE ( 'NONE', #7188, #764, #12318, .T. ) ;
#11259 = DIRECTION ( 'NONE',  ( 0.000000000000000000, 0.000000000000000000, 1.000000000000000000 ) ) ;
#11260 = VECTOR ( 'NONE', #3438, 1000.000000000000000 ) ;
#11261 =( NAMED_UNIT ( * ) PLANE_ANGLE_UNIT ( ) SI_UNIT ( $, .RADIAN. ) );
#11262 = EDGE_CURVE ( 'NONE', #5823, #4652, #9192, .T. ) ;
#11263 = DIRECTION ( 'NONE',  ( 0.000000000000000000, 0.000000000000000000, -1.000000000000000000 ) ) ;
#11264 = DIRECTION ( 'NONE',  ( 0.000000000000000000, 0.000000000000000000, -1.000000000000000000 ) ) ;
#11265 = EDGE_LOOP ( 'NONE', ( #13303, #90, #2694, #9616 ) ) ;
#11266 = ORIENTED_EDGE ( 'NONE', *, *, #13656, .F. ) ;
#11267 = AXIS2_PLACEMENT_3D ( 'NONE', #11173, #996, #1217 ) ;
#11268 = EDGE_LOOP ( 'NONE', ( #5057, #13780, #4991, #13413 ) ) ;
#11269 = LINE ( 'NONE', #11677, #6793 ) ;
#11270 = AXIS2_PLACEMENT_3D ( 'NONE', #9730, #12838, #3130 ) ;
#11271 = ORIENTED_EDGE ( 'NONE', *, *, #10935, .T. ) ;
#11272 = DIRECTION ( 'NONE',  ( 1.000000000000000000, 0.000000000000000000, 0.000000000000000000 ) ) ;
#11273 = FACE_OUTER_BOUND ( 'NONE', #5821, .T. ) ;
#11274 = DIRECTION ( 'NONE',  ( 0.000000000000000000, 3.656775105596099119E-15, -1.000000000000000000 ) ) ;
#11275 = EDGE_CURVE ( 'NONE', #10563, #8882, #12294, .T. ) ;
#11276 = ADVANCED_FACE ( 'NONE', ( #307 ), #8611, .F. ) ;
#11277 = DIRECTION ( 'NONE',  ( 0.000000000000000000, 1.000000000000000000, 0.000000000000000000 ) ) ;
#11278 = DIRECTION ( 'NONE',  ( -1.000000000000000000, -0.000000000000000000, -0.000000000000000000 ) ) ;
#11279 = CIRCLE ( 'NONE', #5035, 9.999999999999980460 ) ;
#11280 = CIRCLE ( 'NONE', #9661, 2.041999999999999815 ) ;
#11281 = LINE ( 'NONE', #6921, #10955 ) ;
#11282 = FACE_BOUND ( 'NONE', #5333, .T. ) ;
#11283 = AXIS2_PLACEMENT_3D ( 'NONE', #10542, #573, #5116 ) ;
#11284 = ORIENTED_EDGE ( 'NONE', *, *, #3753, .F. ) ;
#11285 = ADVANCED_FACE ( 'NONE', ( #13610, #2744 ), #11663, .T. ) ;
#11286 = ADVANCED_FACE ( 'NONE', ( #6001 ), #6147, .T. ) ;
#11287 = AXIS2_PLACEMENT_3D ( 'NONE', #13566, #2486, #2347 ) ;
#11288 = APPLICATION_CONTEXT ( 'automotive_design' ) ;
#11289 = EDGE_CURVE ( 'NONE', #11206, #2766, #14166, .T. ) ;
#11290 = EDGE_CURVE ( 'NONE', #6474, #5358, #7872, .T. ) ;
#11291 = LINE ( 'NONE', #5561, #5360 ) ;
#11292 = CARTESIAN_POINT ( 'NONE',  ( 386.6666666666666288, -20.00000000000000000, 219.8500000000001080 ) ) ;
#11293 = VECTOR ( 'NONE', #12135, 1000.000000000000000 ) ;
#11294 = DIRECTION ( 'NONE',  ( -0.000000000000000000, -0.000000000000000000, -1.000000000000000000 ) ) ;
#11295 = ORIENTED_EDGE ( 'NONE', *, *, #8718, .F. ) ;
#11296 = CIRCLE ( 'NONE', #10364, 5.500000000000005329 ) ;
#11297 = AXIS2_PLACEMENT_3D ( 'NONE', #10452, #407, #3636 ) ;
#11298 = CYLINDRICAL_SURFACE ( 'NONE', #12230, 9.999999999999980460 ) ;
#11299 = B_SPLINE_CURVE_WITH_KNOTS ( 'NONE', 3,
 ( #4514, #14295, #1969, #4231, #11989, #8652 ),
 .UNSPECIFIED., .F., .F.,
 ( 4, 2, 4 ),
 ( -3.640115492410698714E-06, 0.0002066546034003381217, 0.0004169493222930869755 ),
 .UNSPECIFIED. ) ;
#11300 = DIRECTION ( 'NONE',  ( 0.000000000000000000, 0.000000000000000000, -1.000000000000000000 ) ) ;
#11301 = CARTESIAN_POINT ( 'NONE',  ( 386.6666666666666288, -10.00000000000000000, -222.5000000000000853 ) ) ;
#11302 = CIRCLE ( 'NONE', #11754, 0.8509999999999999787 ) ;
#11303 = CIRCLE ( 'NONE', #5969, 9.999999999999980460 ) ;
#11304 = VERTEX_POINT ( 'NONE', #8097 ) ;
#11305 =( GEOMETRIC_REPRESENTATION_CONTEXT ( 3 ) GLOBAL_UNCERTAINTY_ASSIGNED_CONTEXT ( ( #6344 ) ) GLOBAL_UNIT_ASSIGNED_CONTEXT ( ( #6635, #2284, #72 ) ) REPRESENTATION_CONTEXT ( 'NONE', 'WORKASPACE' ) );
#11306 = DIRECTION ( 'NONE',  ( 0.000000000000000000, 0.000000000000000000, 1.000000000000000000 ) ) ;
#11307 = ORIENTED_EDGE ( 'NONE', *, *, #8947, .T. ) ;
#11308 = CARTESIAN_POINT ( 'NONE',  ( 2.712762565639649015, -3.052587955997662306, -3.430618716626630871 ) ) ;
#11309 = ORIENTED_EDGE ( 'NONE', *, *, #3977, .F. ) ;
#11310 = ORIENTED_EDGE ( 'NONE', *, *, #10143, .F. ) ;
#11311 = CARTESIAN_POINT ( 'NONE',  ( 299.9999999999999432, -75.00000000000008527, 186.2999999999999829 ) ) ;
#11312 = CARTESIAN_POINT ( 'NONE',  ( 3.540020015735602765, 2.810662092924382627, -3.602146406945867962 ) ) ;
#11313 = DIRECTION ( 'NONE',  ( 1.000000000000000000, 0.000000000000000000, 0.000000000000000000 ) ) ;
#11314 = VECTOR ( 'NONE', #730, 1000.000000000000000 ) ;
#11315 = FACE_OUTER_BOUND ( 'NONE', #12745, .T. ) ;
#11316 = CARTESIAN_POINT ( 'NONE',  ( -6.259644161404860030E-16, -4.618802153517027165, -3.433295621305388234 ) ) ;
#11317 = DIRECTION ( 'NONE',  ( 1.000000000000000000, 0.000000000000000000, 0.000000000000000000 ) ) ;
#11318 = EDGE_CURVE ( 'NONE', #11433, #11938, #609, .T. ) ;
#11319 = DIRECTION ( 'NONE',  ( -0.000000000000000000, -0.000000000000000000, -1.000000000000000000 ) ) ;
#11320 = ORIENTED_EDGE ( 'NONE', *, *, #10220, .T. ) ;
#11321 = ORIENTED_EDGE ( 'NONE', *, *, #13523, .T. ) ;
#11322 = FACE_OUTER_BOUND ( 'NONE', #10600, .T. ) ;
#11323 = VERTEX_POINT ( 'NONE', #11442 ) ;
#11324 = CARTESIAN_POINT ( 'NONE',  ( 2.500000000000000000, 2.357898499370431722, -2.818925648462311528E-15 ) ) ;
#11325 = VERTEX_POINT ( 'NONE', #9411 ) ;
#11326 = CARTESIAN_POINT ( 'NONE',  ( 2.740000000000000213, 0.000000000000000000, 0.000000000000000000 ) ) ;
#11327 = ORIENTED_EDGE ( 'NONE', *, *, #7456, .F. ) ;
#11328 = AXIS2_PLACEMENT_3D ( 'NONE', #11597, #5084, #691 ) ;
#11329 = DIRECTION ( 'NONE',  ( -1.000000000000000000, -0.000000000000000000, 0.000000000000000000 ) ) ;
#11330 = PRODUCT_DEFINITION_SHAPE ( 'NONE', 'NONE',  #14325 ) ;
#11331 = DIRECTION ( 'NONE',  ( 1.000000000000000000, 0.000000000000000000, 0.000000000000000000 ) ) ;
#11332 = EDGE_LOOP ( 'NONE', ( #10745, #7970 ) ) ;
#11333 = DIRECTION ( 'NONE',  ( 1.000000000000000000, 0.000000000000000000, 0.000000000000000000 ) ) ;
#11334 = DIRECTION ( 'NONE',  ( 1.000000000000000000, 0.000000000000000000, 0.000000000000000000 ) ) ;
#11335 = SURFACE_SIDE_STYLE ('',( #1165 ) ) ;
#11336 = CARTESIAN_POINT ( 'NONE',  ( -2.000000000000006661, 3.464101615137750834, 0.000000000000000000 ) ) ;
#11337 = DIRECTION ( 'NONE',  ( 1.000000000000000000, 0.000000000000000000, 6.123233995736766036E-17 ) ) ;
#11338 = DIRECTION ( 'NONE',  ( -0.000000000000000000, -0.000000000000000000, 1.000000000000000000 ) ) ;
#11339 = VERTEX_POINT ( 'NONE', #9485 ) ;
#11340 = EDGE_LOOP ( 'NONE', ( #11480, #13941, #14030, #137 ) ) ;
#11341 = VERTEX_POINT ( 'NONE', #382 ) ;
#11342 = CARTESIAN_POINT ( 'NONE',  ( 0.000000000000000000, 0.000000000000000000, -0.3080913168122742518 ) ) ;
#11343 = ADVANCED_FACE ( 'NONE', ( #11374, #10505 ), #3972, .F. ) ;
#11344 = ORIENTED_EDGE ( 'NONE', *, *, #3325, .F. ) ;
#11345 = CARTESIAN_POINT ( 'NONE',  ( 145.0000000000000000, 55.00000000000000711, 10.00000000000000000 ) ) ;
#11346 = VERTEX_POINT ( 'NONE', #10429 ) ;
#11347 = DIRECTION ( 'NONE',  ( 1.000000000000000000, 0.000000000000000000, 0.000000000000000000 ) ) ;
#11348 = FACE_OUTER_BOUND ( 'NONE', #6461, .T. ) ;
#11349 = VECTOR ( 'NONE', #1186, 1000.000000000000000 ) ;
#11350 = CARTESIAN_POINT ( 'NONE',  ( -135.0000000000000000, -75.00000000000008527, 40.00000000000000000 ) ) ;
#11351 = AXIS2_PLACEMENT_3D ( 'NONE', #11001, #4407, #5481 ) ;
#11352 = DIRECTION ( 'NONE',  ( -0.000000000000000000, -0.000000000000000000, -1.000000000000000000 ) ) ;
#11353 = DIRECTION ( 'NONE',  ( 0.000000000000000000, -1.000000000000000000, 0.000000000000000000 ) ) ;
#11354 = AXIS2_PLACEMENT_3D ( 'NONE', #5613, #2130, #6559 ) ;
#11355 = CARTESIAN_POINT ( 'NONE',  ( -2.500000000000000888, 0.000000000000000000, -4.974599999999998801 ) ) ;
#11356 = ORIENTED_EDGE ( 'NONE', *, *, #5427, .T. ) ;
#11357 = ADVANCED_FACE ( 'NONE', ( #3901, #8316 ), #2527, .T. ) ;
#11358 = SURFACE_STYLE_USAGE ( .BOTH. , #13740 ) ;
#11359 = CIRCLE ( 'NONE', #5122, 2.041999999999999815 ) ;
#11360 = DIRECTION ( 'NONE',  ( 1.000000000000000000, 0.000000000000000000, 0.000000000000000000 ) ) ;
#11361 = CARTESIAN_POINT ( 'NONE',  ( 0.06760930072668894231, 0.9010842325122832008, -0.5150000000000000133 ) ) ;
#11362 = VERTEX_POINT ( 'NONE', #12597 ) ;
#11363 = CIRCLE ( 'NONE', #2339, 5.500000000000005329 ) ;
#11364 = CARTESIAN_POINT ( 'NONE',  ( -304.9999999999999432, 45.00000000000001421, 40.00000000000000000 ) ) ;
#11365 = EDGE_CURVE ( 'NONE', #9162, #10535, #2664, .T. ) ;
#11366 = ADVANCED_FACE ( 'NONE', ( #458 ), #13903, .F. ) ;
#11367 = CARTESIAN_POINT ( 'NONE',  ( 2.500000000000000000, -1.178949249685213863, 2.042000000000002924 ) ) ;
#11368 = DIRECTION ( 'NONE',  ( 1.000000000000000000, 0.000000000000000000, 0.000000000000000000 ) ) ;
#11369 = AXIS2_PLACEMENT_3D ( 'NONE', #6595, #11022, #1052 ) ;
#11370 = AXIS2_PLACEMENT_3D ( 'NONE', #2576, #9464, #6993 ) ;
#11371 = VERTEX_POINT ( 'NONE', #6513 ) ;
#11372 = DIRECTION ( 'NONE',  ( 0.000000000000000000, 1.000000000000000000, 0.000000000000000000 ) ) ;
#11373 = VERTEX_POINT ( 'NONE', #2890 ) ;
#11374 = FACE_OUTER_BOUND ( 'NONE', #10834, .T. ) ;
#11375 = VECTOR ( 'NONE', #12964, 1000.000000000000000 ) ;
#11376 = VERTEX_POINT ( 'NONE', #14255 ) ;
#11377 = ORIENTED_EDGE ( 'NONE', *, *, #11290, .F. ) ;
#11378 = CYLINDRICAL_SURFACE ( 'NONE', #828, 5.500000000000005329 ) ;
#11379 = CARTESIAN_POINT ( 'NONE',  ( 0.6810597143197052450, 4.461075778259290914, -3.598441714920602053 ) ) ;
#11380 = DIRECTION ( 'NONE',  ( -1.000000000000000000, 0.000000000000000000, 0.000000000000000000 ) ) ;
#11381 = MECHANICAL_DESIGN_GEOMETRIC_PRESENTATION_REPRESENTATION (  '', ( #672 ), #7419 ) ;
#11382 = EDGE_CURVE ( 'NONE', #8368, #12612, #9781, .T. ) ;
#11383 = DIRECTION ( 'NONE',  ( 0.000000000000000000, -1.000000000000000000, 0.000000000000000000 ) ) ;
#11384 = LINE ( 'NONE', #8924, #7905 ) ;
#11385 = DIRECTION ( 'NONE',  ( -0.000000000000000000, -0.000000000000000000, -1.000000000000000000 ) ) ;
#11386 =( NAMED_UNIT ( * ) PLANE_ANGLE_UNIT ( ) SI_UNIT ( $, .RADIAN. ) );
#11387 = EDGE_CURVE ( 'NONE', #1708, #2928, #10728, .T. ) ;
#11388 = CARTESIAN_POINT ( 'NONE',  ( 386.6666666666666288, -20.00000000000000000, 222.5000000000000853 ) ) ;
#11389 = CONTEXT_DEPENDENT_SHAPE_REPRESENTATION ( #10686, #2889 ) ;
#11390 = CIRCLE ( 'NONE', #1874, 2.500000000000002220 ) ;
#11391 = ORIENTED_EDGE ( 'NONE', *, *, #9349, .F. ) ;
#11392 = EDGE_LOOP ( 'NONE', ( #3492, #1598, #7829, #14273, #5814, #11803, #14112, #5942, #13623, #11773, #8112, #809, #6386 ) ) ;
#11393 = ADVANCED_FACE ( 'NONE', ( #2080 ), #4194, .F. ) ;
#11394 = CARTESIAN_POINT ( 'NONE',  ( 2.500000000000000000, 0.000000000000000000, 2.041999999999999815 ) ) ;
#11395 = ORIENTED_EDGE ( 'NONE', *, *, #7099, .F. ) ;
#11396 = DIRECTION ( 'NONE',  ( -0.000000000000000000, -0.000000000000000000, -1.000000000000000000 ) ) ;
#11397 = ORIENTED_EDGE ( 'NONE', *, *, #10293, .T. ) ;
#11398 = FACE_OUTER_BOUND ( 'NONE', #7363, .T. ) ;
#11399 = ORIENTED_EDGE ( 'NONE', *, *, #4794, .F. ) ;
#11400 = CYLINDRICAL_SURFACE ( 'NONE', #1286, 10.00000000000000888 ) ;
#11401 = DIRECTION ( 'NONE',  ( -0.5000000000000051070, 0.000000000000000000, 0.8660254037844355990 ) ) ;
#11403 = VERTEX_POINT ( 'NONE', #5146 ) ;
#11402 = CIRCLE ( 'NONE', #241, 2.500000000000002220 ) ;
#11404 = CARTESIAN_POINT ( 'NONE',  ( 203.5000000000000000, -85.00000000000007105, 55.00000000000001421 ) ) ;
#11405 = DIRECTION ( 'NONE',  ( 0.000000000000000000, 0.000000000000000000, 1.000000000000000000 ) ) ;
#11406 = AXIS2_PLACEMENT_3D ( 'NONE', #7871, #13258, #2086 ) ;
#11407 = DIRECTION ( 'NONE',  ( 1.000000000000000000, 0.000000000000000000, 0.000000000000000000 ) ) ;
#11408 = APPLICATION_PROTOCOL_DEFINITION ( 'draft international standard', 'automotive_design', 1998, #4152 ) ;
#11409 = DIRECTION ( 'NONE',  ( -1.000000000000000000, -0.000000000000000000, -0.000000000000000000 ) ) ;
#11410 = ORIENTED_EDGE ( 'NONE', *, *, #4998, .F. ) ;
#11411 = ORIENTED_EDGE ( 'NONE', *, *, #13899, .F. ) ;
#11412 = ORIENTED_EDGE ( 'NONE', *, *, #6843, .T. ) ;
#11413 = FACE_OUTER_BOUND ( 'NONE', #2152, .T. ) ;
#11414 = ORIENTED_EDGE ( 'NONE', *, *, #7359, .F. ) ;
#11415 = ADVANCED_FACE ( 'NONE', ( #4121 ), #9779, .T. ) ;
#11416 = ORIENTED_EDGE ( 'NONE', *, *, #2606, .F. ) ;
#11417 = CARTESIAN_POINT ( 'NONE',  ( 8.000000000000000000, -4.837354856632045452E-15, 0.000000000000000000 ) ) ;
#11418 = VECTOR ( 'NONE', #6237, 999.9999999999998863 ) ;
#11419 = ORIENTED_EDGE ( 'NONE', *, *, #2758, .F. ) ;
#11420 = DIRECTION ( 'NONE',  ( -0.000000000000000000, -0.000000000000000000, 1.000000000000000000 ) ) ;
#11421 = DIRECTION ( 'NONE',  ( -1.000000000000000000, -0.000000000000000000, -0.000000000000000000 ) ) ;
#11422 =( REPRESENTATION_RELATIONSHIP ('NONE','NONE', #11251, #7730 ) REPRESENTATION_RELATIONSHIP_WITH_TRANSFORMATION ( #7389 )SHAPE_REPRESENTATION_RELATIONSHIP( ) );
#11423 = CARTESIAN_POINT ( 'NONE',  ( 299.9999999999999432, -95.00000000000008527, 169.9999999999999716 ) ) ;
#11424 = AXIS2_PLACEMENT_3D ( 'NONE', #7502, #739, #12727 ) ;
#11425 = DIRECTION ( 'NONE',  ( 1.000000000000000000, 0.000000000000000000, 0.000000000000000000 ) ) ;
#11426 = FACE_OUTER_BOUND ( 'NONE', #6750, .T. ) ;
#11427 = B_SPLINE_CURVE_WITH_KNOTS ( 'NONE', 3,
 ( #1883, #10746, #10814, #9365, #13776, #3843, #2760, #6930 ),
 .UNSPECIFIED., .F., .F.,
 ( 4, 2, 2, 4 ),
 ( 0.000000000000000000, 0.002450665683189820997, 0.003675998524784731495, 0.004901331366379641993 ),
 .UNSPECIFIED. ) ;
#11428 = DIRECTION ( 'NONE',  ( 0.000000000000000000, -0.000000000000000000, 1.000000000000000000 ) ) ;
#11429 = FACE_BOUND ( 'NONE', #6959, .T. ) ;
#11430 = ORIENTED_EDGE ( 'NONE', *, *, #6889, .T. ) ;
#11431 = DIRECTION ( 'NONE',  ( -0.000000000000000000, -0.000000000000000000, 1.000000000000000000 ) ) ;
#11432 = CARTESIAN_POINT ( 'NONE',  ( 53.33333333333330017, -15.00000000000000000, 222.5000000000000853 ) ) ;
#11433 = VERTEX_POINT ( 'NONE', #5215 ) ;
#11434 = DIRECTION ( 'NONE',  ( -0.000000000000000000, 1.000000000000000000, -0.000000000000000000 ) ) ;
#11435 = EDGE_CURVE ( 'NONE', #4062, #9311, #4915, .T. ) ;
#11436 = DIRECTION ( 'NONE',  ( 0.000000000000000000, 0.000000000000000000, -1.000000000000000000 ) ) ;
#11437 = CARTESIAN_POINT ( 'NONE',  ( 439.9999999999999432, 0.000000000000000000, 0.000000000000000000 ) ) ;
#11438 = EDGE_CURVE ( 'NONE', #3406, #6981, #4265, .T. ) ;
#11439 = DIRECTION ( 'NONE',  ( -1.000000000000000000, 0.000000000000000000, 0.000000000000000000 ) ) ;
#11440 = ORIENTED_EDGE ( 'NONE', *, *, #10858, .F. ) ;
#11441 = PRODUCT ( 'socket head cap screw_iso_ISO 4762 M5 x 20 - 20N', 'socket head cap screw_iso_ISO 4762 M5 x 20 - 20N', '', ( #414 ) ) ;
#11442 = CARTESIAN_POINT ( 'NONE',  ( -4.000000000000000000, 2.309401076758498483, -0.4999999999999927280 ) ) ;
#11443 = EDGE_CURVE ( 'NONE', #7589, #4114, #5424, .T. ) ;
#11444 = ORIENTED_EDGE ( 'NONE', *, *, #6248, .T. ) ;
#11445 = DIRECTION ( 'NONE',  ( -0.000000000000000000, -0.000000000000000000, -1.000000000000000000 ) ) ;
#11446 = CARTESIAN_POINT ( 'NONE',  ( 3.453038570460273071, 2.625189405340834448, -3.535263753543585352 ) ) ;
#11447 = CARTESIAN_POINT ( 'NONE',  ( 386.6666666666666288, -20.00000000000000000, 225.1500000000000625 ) ) ;
#11448 = EDGE_CURVE ( 'NONE', #11751, #5872, #9563, .T. ) ;
#11449 = DIRECTION ( 'NONE',  ( 0.000000000000000000, 0.000000000000000000, 1.000000000000000000 ) ) ;
#11450 = ADVANCED_FACE ( 'NONE', ( #1862, #11735 ), #6285, .F. ) ;
#11451 = CARTESIAN_POINT ( 'NONE',  ( 134.9999999999999432, -36.99999999999997868, -181.5021515430661054 ) ) ;
#11452 = CARTESIAN_POINT ( 'NONE',  ( 2.500000000000000000, 2.357898499370431722, -2.818925648462311528E-15 ) ) ;
#11453 =( LENGTH_UNIT ( ) NAMED_UNIT ( * ) SI_UNIT ( .MILLI., .METRE. ) );
#11454 = CYLINDRICAL_SURFACE ( 'NONE', #6703, 2.649999999999985700 ) ;
#11455 = CONTEXT_DEPENDENT_SHAPE_REPRESENTATION ( #12704, #6125 ) ;
#11456 = ORIENTED_EDGE ( 'NONE', *, *, #5848, .T. ) ;
#11457 = ORIENTED_EDGE ( 'NONE', *, *, #10206, .F. ) ;
#11458 = DIRECTION ( 'NONE',  ( 1.000000000000000000, 0.000000000000000000, 0.000000000000000000 ) ) ;
#11459 = EDGE_LOOP ( 'NONE', ( #3550, #1902, #13094, #3053 ) ) ;
#11460 = DIRECTION ( 'NONE',  ( 0.000000000000000000, -0.000000000000000000, 1.000000000000000000 ) ) ;
#11461 = EDGE_CURVE ( 'NONE', #5968, #4187, #2110, .T. ) ;
#11462 = EDGE_CURVE ( 'NONE', #8622, #5874, #5292, .T. ) ;
#11463 = CIRCLE ( 'NONE', #7061, 2.500000000000002220 ) ;
#11464 = CIRCLE ( 'NONE', #84, 10.72499999999999964 ) ;
#11465 = ORIENTED_EDGE ( 'NONE', *, *, #7530, .F. ) ;
#11466 = EDGE_CURVE ( 'NONE', #5335, #11791, #10212, .T. ) ;
#11467 = FACE_OUTER_BOUND ( 'NONE', #10044, .T. ) ;
#11468 = ORIENTED_EDGE ( 'NONE', *, *, #13667, .T. ) ;
#11469 = DIRECTION ( 'NONE',  ( 0.000000000000000000, 1.000000000000000000, -1.287488025362403787E-15 ) ) ;
#11470 = CARTESIAN_POINT ( 'NONE',  ( 2.500000000000000000, 2.357898499370431722, -2.818925648462311528E-15 ) ) ;
#11471 = ORIENTED_EDGE ( 'NONE', *, *, #6302, .T. ) ;
#11472 = CARTESIAN_POINT ( 'NONE',  ( 470.0000000000000000, -15.00000000000000000, 240.0000000000000284 ) ) ;
#11473 = EDGE_CURVE ( 'NONE', #806, #5643, #8540, .T. ) ;
#11474 = CARTESIAN_POINT ( 'NONE',  ( 2.500000000000000000, -1.178949249685214307, 2.042000000000001592 ) ) ;
#11475 = APPLICATION_PROTOCOL_DEFINITION ( 'draft international standard', 'automotive_design', 1998, #10266 ) ;
#11476 = FACE_BOUND ( 'NONE', #8638, .T. ) ;
#11477 = CIRCLE ( 'NONE', #11015, 2.649999999999985700 ) ;
#11478 = ORIENTED_EDGE ( 'NONE', *, *, #14251, .T. ) ;
#11479 = ORIENTED_EDGE ( 'NONE', *, *, #8504, .F. ) ;
#11480 = ORIENTED_EDGE ( 'NONE', *, *, #11633, .F. ) ;
#11481 = CARTESIAN_POINT ( 'NONE',  ( 1.567478505476134606E-15, 4.618802153517012066, -3.433295621305382905 ) ) ;
#11482 = ORIENTED_EDGE ( 'NONE', *, *, #8607, .T. ) ;
#11483 = CARTESIAN_POINT ( 'NONE',  ( -5.000000000000000888, 8.660254037844390851, 210.0000000000000000 ) ) ;
#11484 = ORIENTED_EDGE ( 'NONE', *, *, #10271, .F. ) ;
#11485 = LINE ( 'NONE', #5977, #6865 ) ;
#11486 = AXIS2_PLACEMENT_3D ( 'NONE', #13922, #5016, #6024 ) ;
#11487 = LINE ( 'NONE', #6120, #3224 ) ;
#11488 = CARTESIAN_POINT ( 'NONE',  ( 0.000000000000000000, 0.000000000000000000, -5.000000000000000888 ) ) ;
#11489 = AXIS2_PLACEMENT_3D ( 'NONE', #9722, #13110, #14125 ) ;
#11490 = DIRECTION ( 'NONE',  ( -0.8571673013836870192, 1.049727191973306873E-16, 0.5150380737757234151 ) ) ;
#11491 = CARTESIAN_POINT ( 'NONE',  ( 134.9999999999999432, -56.99999999999997158, -180.0000000000000000 ) ) ;
#11492 = DIRECTION ( 'NONE',  ( -0.000000000000000000, -0.000000000000000000, 1.000000000000000000 ) ) ;
#11493 = CARTESIAN_POINT ( 'NONE',  ( -1.800000000000002931, 1.653273178848927064E-15, 13.50000000000000355 ) ) ;
#11494 = ADVANCED_FACE ( 'NONE', ( #10652 ), #7518, .F. ) ;
#11495 = VERTEX_POINT ( 'NONE', #6365 ) ;
#11496 = VECTOR ( 'NONE', #1060, 1000.000000000000000 ) ;
#11497 = VECTOR ( 'NONE', #13923, 1000.000000000000000 ) ;
#11498 =( REPRESENTATION_RELATIONSHIP ('NONE','NONE', #11251, #11637 ) REPRESENTATION_RELATIONSHIP_WITH_TRANSFORMATION ( #13480 )SHAPE_REPRESENTATION_RELATIONSHIP( ) );
#11499 = CYLINDRICAL_SURFACE ( 'NONE', #971, 5.000000000000004441 ) ;
#11500 = DIRECTION ( 'NONE',  ( -0.000000000000000000, -0.000000000000000000, 1.000000000000000000 ) ) ;
#11501 = DIRECTION ( 'NONE',  ( 0.000000000000000000, 0.000000000000000000, -1.000000000000000000 ) ) ;
#11502 = AXIS2_PLACEMENT_3D ( 'NONE', #13275, #6814, #6745 ) ;
#11503 = EDGE_LOOP ( 'NONE', ( #5542, #3218, #911, #7340 ) ) ;
#11504 = CIRCLE ( 'NONE', #7567, 2.649999999999985700 ) ;
#11505 = AXIS2_PLACEMENT_3D ( 'NONE', #6653, #11089, #5833 ) ;
#11506 = DIRECTION ( 'NONE',  ( -0.000000000000000000, -0.000000000000000000, -1.000000000000000000 ) ) ;
#11507 = CIRCLE ( 'NONE', #10109, 2.649999999999985700 ) ;
#11508 = FACE_OUTER_BOUND ( 'NONE', #11701, .T. ) ;
#11509 = CARTESIAN_POINT ( 'NONE',  ( 176.0000000000000000, 0.000000000000000000, 0.000000000000000000 ) ) ;
#11510 = FACE_OUTER_BOUND ( 'NONE', #196, .T. ) ;
#11511 = ORIENTED_EDGE ( 'NONE', *, *, #13158, .T. ) ;
#11512 = CARTESIAN_POINT ( 'NONE',  ( 17.00000000000000000, 0.000000000000000000, 0.000000000000000000 ) ) ;
#11513 = AXIS2_PLACEMENT_3D ( 'NONE', #8800, #4241, #3160 ) ;
#11514 = DIRECTION ( 'NONE',  ( 1.000000000000000000, 0.000000000000000000, 0.000000000000000000 ) ) ;
#11515 = EDGE_CURVE ( 'NONE', #6665, #5470, #2002, .T. ) ;
#11516 = AXIS2_PLACEMENT_3D ( 'NONE', #10375, #2472, #6897 ) ;
#11517 = VECTOR ( 'NONE', #1087, 1000.000000000000000 ) ;
#11518 = VERTEX_POINT ( 'NONE', #10196 ) ;
#11519 = CARTESIAN_POINT ( 'NONE',  ( -314.9999999999999432, -105.0000000000000995, 40.00000000000000000 ) ) ;
#11520 = CARTESIAN_POINT ( 'NONE',  ( 0.02511973781850649831, -4.877415612947427981, -3.751298745799844792 ) ) ;
#11521 = AXIS2_PLACEMENT_3D ( 'NONE', #3512, #1240, #2414 ) ;
#11522 = CARTESIAN_POINT ( 'NONE',  ( 386.6666666666666288, -20.00000000000000000, -222.5000000000000853 ) ) ;
#11523 = DIRECTION ( 'NONE',  ( 0.000000000000000000, 0.000000000000000000, 1.000000000000000000 ) ) ;
#11524 = DIRECTION ( 'NONE',  ( -0.000000000000000000, -0.000000000000000000, -1.000000000000000000 ) ) ;
#11525 = DIRECTION ( 'NONE',  ( 0.000000000000000000, 0.4999999999999992784, -0.8660254037844389297 ) ) ;
#11526 = FACE_OUTER_BOUND ( 'NONE', #4741, .T. ) ;
#11527 = CONTEXT_DEPENDENT_SHAPE_REPRESENTATION ( #4279, #12046 ) ;
#11528 = AXIS2_PLACEMENT_3D ( 'NONE', #520, #4982, #10562 ) ;
#11529 = ORIENTED_EDGE ( 'NONE', *, *, #8902, .F. ) ;
#11530 = ORIENTED_EDGE ( 'NONE', *, *, #6117, .F. ) ;
#11531 = CYLINDRICAL_SURFACE ( 'NONE', #1978, 2.649999999999985700 ) ;
#11532 = ORIENTED_EDGE ( 'NONE', *, *, #5065, .F. ) ;
#11533 = CARTESIAN_POINT ( 'NONE',  ( -5.000000000000000888, -8.660254037844389075, 210.0000000000000000 ) ) ;
#11534 = DIRECTION ( 'NONE',  ( -0.000000000000000000, 0.000000000000000000, 1.000000000000000000 ) ) ;
#11535 = EDGE_CURVE ( 'NONE', #6820, #3349, #12303, .T. ) ;
#11536 = AXIS2_PLACEMENT_3D ( 'NONE', #11958, #12895, #2972 ) ;
#11537 = ORIENTED_EDGE ( 'NONE', *, *, #9775, .F. ) ;
#11538 = DIRECTION ( 'NONE',  ( 0.8571673013836870192, 0.000000000000000000, 0.5150380737757234151 ) ) ;
#11539 = EDGE_LOOP ( 'NONE', ( #1724, #13811 ) ) ;
#11540 = DIRECTION ( 'NONE',  ( -1.000000000000000000, 0.000000000000000000, 0.000000000000000000 ) ) ;
#11541 = VECTOR ( 'NONE', #427, 1000.000000000000000 ) ;
#11542 = CYLINDRICAL_SURFACE ( 'NONE', #5727, 2.649999999999985700 ) ;
#11543 = ORIENTED_EDGE ( 'NONE', *, *, #10763, .F. ) ;
#11544 = FACE_OUTER_BOUND ( 'NONE', #8350, .T. ) ;
#11545 = APPLICATION_PROTOCOL_DEFINITION ( 'draft international standard', 'automotive_design', 1998, #13047 ) ;
#11546 = EDGE_CURVE ( 'NONE', #8111, #9222, #13235, .T. ) ;
#11547 = EDGE_CURVE ( 'NONE', #8744, #10991, #10920, .T. ) ;
#11548 = CARTESIAN_POINT ( 'NONE',  ( -4.000000000000000000, 2.309401076758498483, -3.433295621305379353 ) ) ;
#11549 = VERTEX_POINT ( 'NONE', #11086 ) ;
#11550 = EDGE_CURVE ( 'NONE', #13194, #11433, #13380, .T. ) ;
#11551 = ORIENTED_EDGE ( 'NONE', *, *, #62, .T. ) ;
#11552 = VERTEX_POINT ( 'NONE', #4485 ) ;
#11553 = CARTESIAN_POINT ( 'NONE',  ( 4.000000000000000000, -2.309401076758516691, -0.4999999999999995559 ) ) ;
#11554 = VECTOR ( 'NONE', #8546, 1000.000000000000000 ) ;
#11555 = VERTEX_POINT ( 'NONE', #2368 ) ;
#11556 = DIRECTION ( 'NONE',  ( 0.000000000000000000, -1.000000000000000000, 1.471414886128461471E-15 ) ) ;
#11557 = ORIENTED_EDGE ( 'NONE', *, *, #10853, .F. ) ;
#11558 = DIRECTION ( 'NONE',  ( -1.000000000000000000, -0.000000000000000000, -0.000000000000000000 ) ) ;
#11559 = CARTESIAN_POINT ( 'NONE',  ( 0.000000000000000000, 15.00000000000000000, 200.0000000000000000 ) ) ;
#11560 = CARTESIAN_POINT ( 'NONE',  ( 236.4999999999999432, -85.00000000000007105, 180.0000000000000000 ) ) ;
#11561 = APPLICATION_CONTEXT ( 'automotive_design' ) ;
#11562 = LINE ( 'NONE', #510, #12088 ) ;
#11563 = FACE_OUTER_BOUND ( 'NONE', #8795, .T. ) ;
#11564 = AXIS2_PLACEMENT_3D ( 'NONE', #13541, #2395, #1570 ) ;
#11565 = CARTESIAN_POINT ( 'NONE',  ( 2.500000000000000000, 2.357898499370433054, -1.951563910473907981E-15 ) ) ;
#11566 = PRODUCT_DEFINITION_SHAPE ( 'NONE', 'NONE',  #14382 ) ;
#11567 = EDGE_CURVE ( 'NONE', #11339, #14007, #6961, .T. ) ;
#11568 = ORIENTED_EDGE ( 'NONE', *, *, #6511, .F. ) ;
#11569 = VERTEX_POINT ( 'NONE', #8963 ) ;
#11570 = ORIENTED_EDGE ( 'NONE', *, *, #7868, .F. ) ;
#11571 = CARTESIAN_POINT ( 'NONE',  ( -30.00000000000002842, -25.00000000000000000, 250.0000000000000000 ) ) ;
#11572 = AXIS2_PLACEMENT_3D ( 'NONE', #4110, #13969, #12737 ) ;
#11573 = CARTESIAN_POINT ( 'NONE',  ( 170.9999999999999716, -8.660254037844389075, 199.9990000000000236 ) ) ;
#11574 = SURFACE_STYLE_FILL_AREA ( #7146 ) ;
#11575 = EDGE_CURVE ( 'NONE', #12771, #3344, #11291, .T. ) ;
#11576 = ORIENTED_EDGE ( 'NONE', *, *, #238, .T. ) ;
#11577 = DIRECTION ( 'NONE',  ( 1.000000000000000000, 0.000000000000000000, 0.000000000000000000 ) ) ;
#11578 = CARTESIAN_POINT ( 'NONE',  ( 142.6500000000000057, -95.00000000000008527, -186.2999999999999829 ) ) ;
#11579 = CARTESIAN_POINT ( 'NONE',  ( 352.0000000000000000, 0.000000000000000000, 0.000000000000000000 ) ) ;
#11580 = FACE_OUTER_BOUND ( 'NONE', #10918, .T. ) ;
#11581 = CARTESIAN_POINT ( 'NONE',  ( 136.6666666666666288, -15.00000000000000000, 219.8500000000001080 ) ) ;
#11582 = AXIS2_PLACEMENT_3D ( 'NONE', #7230, #2888, #11662 ) ;
#11583 = CIRCLE ( 'NONE', #5344, 2.649999999999985700 ) ;
#11584 = EDGE_LOOP ( 'NONE', ( #3074, #11722, #4714, #3327 ) ) ;
#11585 = SPHERICAL_SURFACE ( 'NONE', #12976, 8.000000000000000000 ) ;
#11586 = CONICAL_SURFACE ( 'NONE', #13433, 2.055000000000000160, 0.7853981633974721488 ) ;
#11587 = DIRECTION ( 'NONE',  ( 0.000000000000000000, 0.000000000000000000, -1.000000000000000000 ) ) ;
#11588 = EDGE_CURVE ( 'NONE', #1964, #4974, #13679, .T. ) ;
#11589 = ORIENTED_EDGE ( 'NONE', *, *, #4868, .T. ) ;
#11590 = CARTESIAN_POINT ( 'NONE',  ( 28.70000000000000284, 0.000000000000000000, 0.000000000000000000 ) ) ;
#11591 = AXIS2_PLACEMENT_3D ( 'NONE', #1486, #4774, #11514 ) ;
#11592 = AXIS2_PLACEMENT_3D ( 'NONE', #4264, #8609, #5423 ) ;
#11593 = LINE ( 'NONE', #8394, #9758 ) ;
#11594 = CARTESIAN_POINT ( 'NONE',  ( 181.0000000000000000, 8.660254037844390851, 199.9990000000000236 ) ) ;
#11595 = DIRECTION ( 'NONE',  ( -0.000000000000000000, -0.000000000000000000, 1.000000000000000000 ) ) ;
#11596 = VECTOR ( 'NONE', #11215, 1000.000000000000000 ) ;
#11597 = CARTESIAN_POINT ( 'NONE',  ( 305.0000000000000000, -36.99999999999997868, -180.0000000000000000 ) ) ;
#11598 = EDGE_CURVE ( 'NONE', #4143, #6597, #686, .T. ) ;
#11599 = ITEM_DEFINED_TRANSFORMATION ( 'NONE', 'NONE', #7462,  #14039 ) ;
#11600 = VERTEX_POINT ( 'NONE', #11149 ) ;
#11601 = CARTESIAN_POINT ( 'NONE',  ( -140.0000000000000000, -75.00000000000008527, -14.14213562373090127 ) ) ;
#11602 = AXIS2_PLACEMENT_3D ( 'NONE', #7660, #7795, #12231 ) ;
#11603 = ORIENTED_EDGE ( 'NONE', *, *, #12376, .T. ) ;
#11604 = DIRECTION ( 'NONE',  ( -0.000000000000000000, -1.000000000000000000, -0.000000000000000000 ) ) ;
#11605 = DIRECTION ( 'NONE',  ( 1.000000000000000000, 0.000000000000000000, 0.000000000000000000 ) ) ;
#11606 = ORIENTED_EDGE ( 'NONE', *, *, #3817, .F. ) ;
#11607 = CARTESIAN_POINT ( 'NONE',  ( 319.9999999999999432, -24.99999999999999289, -19.99999999999998934 ) ) ;
#11608 = VERTEX_POINT ( 'NONE', #2220 ) ;
#11609 = AXIS2_PLACEMENT_3D ( 'NONE', #7064, #8214, #511 ) ;
#11610 = CYLINDRICAL_SURFACE ( 'NONE', #6150, 2.649999999999985700 ) ;
#11611 = CARTESIAN_POINT ( 'NONE',  ( -4.203833317240879275, -1.627343821129593859, -3.597273115243890818 ) ) ;
#11612 = ORIENTED_EDGE ( 'NONE', *, *, #4277, .T. ) ;
#11613 = UNCERTAINTY_MEASURE_WITH_UNIT (LENGTH_MEASURE( 1.000000000000000082E-05 ), #6373, 'distance_accuracy_value', 'NONE');
#11614 = LINE ( 'NONE', #13782, #1326 ) ;
#11615 = CARTESIAN_POINT ( 'NONE',  ( 134.9999999999999716, 45.00000000000001421, 10.00000000000000000 ) ) ;
#11616 =( NAMED_UNIT ( * ) PLANE_ANGLE_UNIT ( ) SI_UNIT ( $, .RADIAN. ) );
#11617 = PRESENTATION_STYLE_ASSIGNMENT (( #5889 ) ) ;
#11618 = ADVANCED_FACE ( 'NONE', ( #1114 ), #3462, .F. ) ;
#11619 = APPLICATION_PROTOCOL_DEFINITION ( 'draft international standard', 'automotive_design', 1998, #10074 ) ;
#11620 = CYLINDRICAL_SURFACE ( 'NONE', #4115, 2.500000000000002220 ) ;
#11621 = EDGE_CURVE ( 'NONE', #1677, #14253, #1189, .T. ) ;
#11622 = ORIENTED_EDGE ( 'NONE', *, *, #6581, .T. ) ;
#11623 = EDGE_LOOP ( 'NONE', ( #2075, #13914, #944, #12733 ) ) ;
#11624 = CARTESIAN_POINT ( 'NONE',  ( 20.55500000000001748, 0.000000000000000000, 0.000000000000000000 ) ) ;
#11625 = ORIENTED_EDGE ( 'NONE', *, *, #188, .F. ) ;
#11626 = LINE ( 'NONE', #10762, #7427 ) ;
#11627 = VECTOR ( 'NONE', #8031, 1000.000000000000000 ) ;
#11628 = VECTOR ( 'NONE', #4275, 1000.000000000000000 ) ;
#11629 = ORIENTED_EDGE ( 'NONE', *, *, #5962, .T. ) ;
#11630 = CARTESIAN_POINT ( 'NONE',  ( 21.00000000000000355, 0.000000000000000000, 2.055000000000000160 ) ) ;
#11631 = ORIENTED_EDGE ( 'NONE', *, *, #10934, .F. ) ;
#11632 = FACE_OUTER_BOUND ( 'NONE', #1573, .T. ) ;
#11633 = EDGE_CURVE ( 'NONE', #498, #7372, #5636, .T. ) ;
#11634 = AXIS2_PLACEMENT_3D ( 'NONE', #9926, #8910, #6589 ) ;
#11635 = DIRECTION ( 'NONE',  ( 0.000000000000000000, -0.4999999999999993894, 0.8660254037844389297 ) ) ;
#11636 = DIRECTION ( 'NONE',  ( 0.000000000000000000, -0.000000000000000000, 1.000000000000000000 ) ) ;
#11637 = SHAPE_REPRESENTATION ( 'roller', ( #14039 ), #4925 ) ;
#11638 = DIRECTION ( 'NONE',  ( 1.000000000000000000, 0.000000000000000000, 0.000000000000000000 ) ) ;
#11639 = CARTESIAN_POINT ( 'NONE',  ( 305.4999999999999432, -95.00000000000008527, -190.0000000000000000 ) ) ;
#11640 = EDGE_CURVE ( 'NONE', #5038, #3114, #13250, .T. ) ;
#11641 = CARTESIAN_POINT ( 'NONE',  ( 299.9999999999999432, -75.00000000000008527, 190.0000000000000000 ) ) ;
#11642 = VECTOR ( 'NONE', #13885, 1000.000000000000000 ) ;
#11643 = ORIENTED_EDGE ( 'NONE', *, *, #14102, .F. ) ;
#11644 = ORIENTED_EDGE ( 'NONE', *, *, #9490, .F. ) ;
#11645 = AXIS2_PLACEMENT_3D ( 'NONE', #4111, #4987, #8530 ) ;
#11646 =( GEOMETRIC_REPRESENTATION_CONTEXT ( 3 ) GLOBAL_UNCERTAINTY_ASSIGNED_CONTEXT ( ( #708 ) ) GLOBAL_UNIT_ASSIGNED_CONTEXT ( ( #11198, #5672, #8804 ) ) REPRESENTATION_CONTEXT ( 'NONE', 'WORKASPACE' ) );
#11647 = FACE_OUTER_BOUND ( 'NONE', #6283, .T. ) ;
#11648 = FACE_OUTER_BOUND ( 'NONE', #7141, .T. ) ;
#11649 = DIRECTION ( 'NONE',  ( 0.000000000000000000, -1.000000000000000000, 0.000000000000000000 ) ) ;
#11650 = EDGE_CURVE ( 'NONE', #13280, #2338, #8827, .T. ) ;
#11651 = AXIS2_PLACEMENT_3D ( 'NONE', #9617, #3020, #11865 ) ;
#11652 = ORIENTED_EDGE ( 'NONE', *, *, #4750, .T. ) ;
#11653 = EDGE_CURVE ( 'NONE', #7893, #1312, #6272, .T. ) ;
#11654 = DIRECTION ( 'NONE',  ( 1.007709689656716938E-16, 1.000000000000000000, 3.606821995490528048E-15 ) ) ;
#11655 = CARTESIAN_POINT ( 'NONE',  ( 140.0000000000000000, -75.00000000000008527, -186.2999999999999829 ) ) ;
#11656 = EDGE_CURVE ( 'NONE', #10068, #2665, #9031, .T. ) ;
#11657 = FACE_OUTER_BOUND ( 'NONE', #4370, .T. ) ;
#11658 = DIRECTION ( 'NONE',  ( 0.000000000000000000, 0.000000000000000000, 1.000000000000000000 ) ) ;
#11659 = CARTESIAN_POINT ( 'NONE',  ( 0.000000000000000000, 0.000000000000000000, -200.0000000000000000 ) ) ;
#11660 = DIRECTION ( 'NONE',  ( 0.000000000000000000, 1.000000000000000000, 0.000000000000000000 ) ) ;
#11661 = ORIENTED_EDGE ( 'NONE', *, *, #8296, .T. ) ;
#11662 = DIRECTION ( 'NONE',  ( 1.000000000000000000, 0.000000000000000000, 0.000000000000000000 ) ) ;
#11663 = PLANE ( 'NONE',  #6067 ) ;
#11664 = EDGE_LOOP ( 'NONE', ( #5097, #9728, #3515, #707, #13070 ) ) ;
#11665 = LINE ( 'NONE', #3690, #7096 ) ;
#11666 = DIRECTION ( 'NONE',  ( 0.000000000000000000, 0.000000000000000000, -1.000000000000000000 ) ) ;
#11667 = ADVANCED_FACE ( 'NONE', ( #3257 ), #12095, .T. ) ;
#11668 = DIRECTION ( 'NONE',  ( 1.000000000000000000, 0.000000000000000000, 0.000000000000000000 ) ) ;
#11669 = DIRECTION ( 'NONE',  ( 1.000000000000000000, 0.000000000000000000, 0.000000000000000000 ) ) ;
#11670 = FACE_BOUND ( 'NONE', #5580, .T. ) ;
#11671 = FILL_AREA_STYLE_COLOUR ( '', #3302 ) ;
#11672 = CARTESIAN_POINT ( 'NONE',  ( -2.712762565639006418, 3.052587955997511759, -3.430618716626627318 ) ) ;
#11673 = EDGE_CURVE ( 'NONE', #8279, #2418, #6975, .T. ) ;
#11674 = VERTEX_POINT ( 'NONE', #9103 ) ;
#11675 = DIRECTION ( 'NONE',  ( 0.000000000000000000, 0.000000000000000000, 1.000000000000000000 ) ) ;
#11676 = ORIENTED_EDGE ( 'NONE', *, *, #12561, .T. ) ;
#11677 = CARTESIAN_POINT ( 'NONE',  ( -137.6499999999999773, 45.00000000000001421, 30.00000000000000000 ) ) ;
#11678 = FACE_OUTER_BOUND ( 'NONE', #12808, .T. ) ;
#11679 = ORIENTED_EDGE ( 'NONE', *, *, #7420, .T. ) ;
#11680 = DIRECTION ( 'NONE',  ( 0.000000000000000000, 0.000000000000000000, 1.000000000000000000 ) ) ;
#11681 = VERTEX_POINT ( 'NONE', #4412 ) ;
#11682 = DIRECTION ( 'NONE',  ( 0.000000000000000000, 1.000000000000000000, 0.000000000000000000 ) ) ;
#11683 = PRODUCT_DEFINITION_SHAPE ( 'NONE', 'NONE',  #14335 ) ;
#11684 = DIRECTION ( 'NONE',  ( -1.000000000000000000, -0.000000000000000000, -0.000000000000000000 ) ) ;
#11685 = VERTEX_POINT ( 'NONE', #8220 ) ;
#11686 = FACE_BOUND ( 'NONE', #3637, .T. ) ;
#11687 = CARTESIAN_POINT ( 'NONE',  ( 0.000000000000000000, 8.660254037844390851, -200.0000000000000000 ) ) ;
#11688 = FACE_OUTER_BOUND ( 'NONE', #12930, .T. ) ;
#11689 = SHAPE_DEFINITION_REPRESENTATION ( #3685, #9307 ) ;
#11690 = FACE_OUTER_BOUND ( 'NONE', #9585, .T. ) ;
#11691 = EDGE_CURVE ( 'NONE', #5470, #8094, #2572, .T. ) ;
#11692 = VERTEX_POINT ( 'NONE', #3738 ) ;
#11693 =( REPRESENTATION_RELATIONSHIP ('NONE','NONE', #11251, #2275 ) REPRESENTATION_RELATIONSHIP_WITH_TRANSFORMATION ( #14122 )SHAPE_REPRESENTATION_RELATIONSHIP( ) );
#11694 = EDGE_LOOP ( 'NONE', ( #11711, #11679 ) ) ;
#11695 = FACE_OUTER_BOUND ( 'NONE', #3722, .T. ) ;
#11696 = CLOSED_SHELL ( 'NONE', ( #6330, #9406, #13099, #711, #2863, #14028, #1401, #4729, #7207, #6440, #3332, #10773, #7727, #9684, #6369, #12077, #3941, #11667, #9255, #6463, #9502, #13917, #2214, #10249, #4354, #2171, #10778 ) ) ;
#11697 = ORIENTED_EDGE ( 'NONE', *, *, #3049, .T. ) ;
#11698 = CARTESIAN_POINT ( 'NONE',  ( 2.345747346278113987, -3.264484291692503870, -0.01223254789874484924 ) ) ;
#11699 = ORIENTED_EDGE ( 'NONE', *, *, #9972, .T. ) ;
#11700 = LINE ( 'NONE', #4158, #4109 ) ;
#11701 = EDGE_LOOP ( 'NONE', ( #8295, #3005, #3944, #4661, #7488 ) ) ;
#11702 = EDGE_CURVE ( 'NONE', #3025, #5737, #10490, .T. ) ;
#11703 = CARTESIAN_POINT ( 'NONE',  ( 5.200000000000002842, 0.000000000000000000, 2.500000000000000444 ) ) ;
#11704 = EDGE_CURVE ( 'NONE', #11938, #10462, #367, .T. ) ;
#11705 = CARTESIAN_POINT ( 'NONE',  ( 17.00000000000000000, 0.000000000000000000, 0.000000000000000000 ) ) ;
#11706 = DIRECTION ( 'NONE',  ( -0.000000000000000000, -0.000000000000000000, -1.000000000000000000 ) ) ;
#11707 = AXIS2_PLACEMENT_3D ( 'NONE', #4295, #8716, #13136 ) ;
#11708 = CARTESIAN_POINT ( 'NONE',  ( 203.5000000000000000, -85.00000000000007105, 180.0000000000000000 ) ) ;
#11709 = LINE ( 'NONE', #6195, #4900 ) ;
#11710 = LINE ( 'NONE', #1691, #9233 ) ;
#11711 = ORIENTED_EDGE ( 'NONE', *, *, #4828, .T. ) ;
#11712 = ORIENTED_EDGE ( 'NONE', *, *, #2055, .F. ) ;
#11713 = FACE_OUTER_BOUND ( 'NONE', #14272, .T. ) ;
#11714 = AXIS2_PLACEMENT_3D ( 'NONE', #6826, #5535, #5738 ) ;
#11715 = AXIS2_PLACEMENT_3D ( 'NONE', #12981, #7392, #8551 ) ;
#11716 = EDGE_LOOP ( 'NONE', ( #5033, #9308 ) ) ;
#11717 = DIRECTION ( 'NONE',  ( 0.000000000000000000, 1.000000000000000000, 0.000000000000000000 ) ) ;
#11718 = EDGE_CURVE ( 'NONE', #9107, #9676, #10333, .T. ) ;
#11719 = DIRECTION ( 'NONE',  ( 1.000000000000000000, 0.000000000000000000, 0.000000000000000000 ) ) ;
#11720 = EDGE_CURVE ( 'NONE', #1275, #10676, #923, .T. ) ;
#11721 = DIRECTION ( 'NONE',  ( -0.000000000000000000, 0.000000000000000000, 1.000000000000000000 ) ) ;
#11722 = ORIENTED_EDGE ( 'NONE', *, *, #4935, .T. ) ;
#11723 = DIRECTION ( 'NONE',  ( -0.000000000000000000, 1.000000000000000000, -0.000000000000000000 ) ) ;
#11724 = AXIS2_PLACEMENT_3D ( 'NONE', #10012, #3480, #4430 ) ;
#11725 = FACE_OUTER_BOUND ( 'NONE', #6612, .T. ) ;
#11726 = DIRECTION ( 'NONE',  ( -1.000000000000000000, 0.000000000000000000, 6.123233995736766036E-17 ) ) ;
#11727 = DIRECTION ( 'NONE',  ( -1.000000000000000000, -0.000000000000000000, -0.000000000000000000 ) ) ;
#11728 = EDGE_CURVE ( 'NONE', #1332, #574, #441, .T. ) ;
#11729 = ADVANCED_FACE ( 'NONE', ( #11648 ), #8002, .F. ) ;
#11730 = AXIS2_PLACEMENT_3D ( 'NONE', #12839, #5170, #2911 ) ;
#11731 = EDGE_CURVE ( 'NONE', #6238, #4007, #5842, .T. ) ;
#11732 = EDGE_LOOP ( 'NONE', ( #2901, #8409 ) ) ;
#11733 = CARTESIAN_POINT ( 'NONE',  ( -0.3198814748697807464, -4.434118497892185040, -0.3507732604232532969 ) ) ;
#11734 = CIRCLE ( 'NONE', #1283, 0.2000000000000000944 ) ;
#11735 = FACE_OUTER_BOUND ( 'NONE', #12424, .T. ) ;
#11736 = AXIS2_PLACEMENT_3D ( 'NONE', #3338, #7735, #9243 ) ;
#11737 = ORIENTED_EDGE ( 'NONE', *, *, #9735, .F. ) ;
#11738 = DIRECTION ( 'NONE',  ( 0.000000000000000000, 0.000000000000000000, -1.000000000000000000 ) ) ;
#11739 = VECTOR ( 'NONE', #3585, 1000.000000000000000 ) ;
#11740 = CARTESIAN_POINT ( 'NONE',  ( 0.000000000000000000, 15.00000000000000000, 205.0000000000000284 ) ) ;
#11741 = CYLINDRICAL_SURFACE ( 'NONE', #6501, 2.500000000000002220 ) ;
#11742 = DIRECTION ( 'NONE',  ( -0.000000000000000000, -1.000000000000000000, -0.000000000000000000 ) ) ;
#11743 = SHAPE_REPRESENTATION_RELATIONSHIP ( 'NONE' , 'NONE' ,  #10796, #5928 ) ;
#11744 = VECTOR ( 'NONE', #6915, 1000.000000000000000 ) ;
#11745 = CARTESIAN_POINT ( 'NONE',  ( -1.257172072275743346, 3.892973519171203378, -3.433252694550776862 ) ) ;
#11746 = VECTOR ( 'NONE', #9515, 1000.000000000000000 ) ;
#11747 = EDGE_LOOP ( 'NONE', ( #12871, #2761, #12112, #1439 ) ) ;
#11748 = VECTOR ( 'NONE', #1905, 1000.000000000000341 ) ;
#11749 = CARTESIAN_POINT ( 'NONE',  ( 8.673617379884035472E-16, 4.618802153517012954, -5.000000000000000000 ) ) ;
#11750 = CIRCLE ( 'NONE', #6655, 2.055000000000000160 ) ;
#11751 = VERTEX_POINT ( 'NONE', #2729 ) ;
#11752 = DIRECTION ( 'NONE',  ( 0.000000000000000000, 0.000000000000000000, -1.000000000000000000 ) ) ;
#11753 = DIRECTION ( 'NONE',  ( -0.8949343913984144638, 0.000000000000000000, -0.4461977533474923430 ) ) ;
#11754 = AXIS2_PLACEMENT_3D ( 'NONE', #3578, #11409, #13358 ) ;
#11755 =( REPRESENTATION_RELATIONSHIP ('NONE','NONE', #11251, #9307 ) REPRESENTATION_RELATIONSHIP_WITH_TRANSFORMATION ( #1819 )SHAPE_REPRESENTATION_RELATIONSHIP( ) );
#11756 = ORIENTED_EDGE ( 'NONE', *, *, #4171, .F. ) ;
#11757 = DIRECTION ( 'NONE',  ( -0.000000000000000000, -0.000000000000000000, -1.000000000000000000 ) ) ;
#11758 = EDGE_LOOP ( 'NONE', ( #5450, #11915, #12999, #3824 ) ) ;
#11759 = DIRECTION ( 'NONE',  ( 1.000000000000000000, 0.000000000000000000, 0.000000000000000000 ) ) ;
#11760 = VECTOR ( 'NONE', #9657, 1000.000000000000000 ) ;
#11761 = CARTESIAN_POINT ( 'NONE',  ( -4.197393957002303999, -7.773935952363655451E-14, -3.503767560748929810 ) ) ;
#11762 = ORIENTED_EDGE ( 'NONE', *, *, #4954, .F. ) ;
#11763 = UNCERTAINTY_MEASURE_WITH_UNIT (LENGTH_MEASURE( 1.000000000000000082E-05 ), #13639, 'distance_accuracy_value', 'NONE');
#11764 = EDGE_CURVE ( 'NONE', #2488, #12837, #139, .T. ) ;
#11765 = AXIS2_PLACEMENT_3D ( 'NONE', #12375, #4696, #2371 ) ;
#11766 = CARTESIAN_POINT ( 'NONE',  ( 134.9999999999999716, 45.00000000000001421, 0.000000000000000000 ) ) ;
#11767 = CIRCLE ( 'NONE', #2494, 2.041999999999999815 ) ;
#11768 = CARTESIAN_POINT ( 'NONE',  ( -0.7826237921249277196, 1.353234713057825478E-15, 11.05000000000000071 ) ) ;
#11769 = ORIENTED_EDGE ( 'NONE', *, *, #6914, .T. ) ;
#11770 = ORIENTED_EDGE ( 'NONE', *, *, #6144, .F. ) ;
#11771 = CARTESIAN_POINT ( 'NONE',  ( 0.000000000000000000, -8.660254037844389075, -200.0000000000000000 ) ) ;
#11772 = AXIS2_PLACEMENT_3D ( 'NONE', #9128, #10509, #11380 ) ;
#11773 = ORIENTED_EDGE ( 'NONE', *, *, #13931, .F. ) ;
#11774 = CARTESIAN_POINT ( 'NONE',  ( 219.9999999999999716, -85.00000000000007105, 0.000000000000000000 ) ) ;
#11775 = AXIS2_PLACEMENT_3D ( 'NONE', #2732, #297, #4841 ) ;
#11776 = VERTEX_POINT ( 'NONE', #7144 ) ;
#11777 = DIRECTION ( 'NONE',  ( -1.000000000000000000, -0.000000000000000000, -0.000000000000000000 ) ) ;
#11778 = ORIENTED_EDGE ( 'NONE', *, *, #11275, .F. ) ;
#11779 = FACE_BOUND ( 'NONE', #9284, .T. ) ;
#11780 = CARTESIAN_POINT ( 'NONE',  ( -5.000000000000000888, -8.660254037844389075, 210.0000000000000000 ) ) ;
#11781 = CARTESIAN_POINT ( 'NONE',  ( 302.4999999999999432, 45.00000000000001421, 10.00000000000000000 ) ) ;
#11782 = AXIS2_PLACEMENT_3D ( 'NONE', #3930, #561, #8343 ) ;
#11783 = LINE ( 'NONE', #5197, #471 ) ;
#11784 = DIRECTION ( 'NONE',  ( 0.000000000000000000, 1.000000000000000000, -1.224646799147353207E-16 ) ) ;
#11785 = CARTESIAN_POINT ( 'NONE',  ( 4.999999999999999112, 8.660254037844390851, 210.0000000000000000 ) ) ;
#11786 = VERTEX_POINT ( 'NONE', #1699 ) ;
#11787 = AXIS2_PLACEMENT_3D ( 'NONE', #10789, #8452, #2884 ) ;
#11788 = ADVANCED_FACE ( 'NONE', ( #4979 ), #11499, .F. ) ;
#11789 = EDGE_LOOP ( 'NONE', ( #4945, #7072, #2951, #5753 ) ) ;
#11790 = CARTESIAN_POINT ( 'NONE',  ( -1.799999999999996048, 0.000000000000000000, -10.20000000000000107 ) ) ;
#11791 = VERTEX_POINT ( 'NONE', #1473 ) ;
#11792 = DIRECTION ( 'NONE',  ( 1.000000000000000000, 0.000000000000000000, 0.000000000000000000 ) ) ;
#11793 = CARTESIAN_POINT ( 'NONE',  ( 2.500000000000000000, 2.357898499370431722, -2.818925648462311528E-15 ) ) ;
#11794 =( NAMED_UNIT ( * ) PLANE_ANGLE_UNIT ( ) SI_UNIT ( $, .RADIAN. ) );
#11795 = ORIENTED_EDGE ( 'NONE', *, *, #2300, .T. ) ;
#11796 = AXIS2_PLACEMENT_3D ( 'NONE', #2826, #5221, #11815 ) ;
#11797 = DIRECTION ( 'NONE',  ( 0.000000000000000000, 1.000000000000000000, -1.287488025362403787E-15 ) ) ;
#11798 = CARTESIAN_POINT ( 'NONE',  ( 2.000000000000001776, 0.000000000000000000, 0.000000000000000000 ) ) ;
#11799 = DIRECTION ( 'NONE',  ( 0.000000000000000000, 0.000000000000000000, 1.000000000000000000 ) ) ;
#11800 = DIRECTION ( 'NONE',  ( -0.000000000000000000, -0.000000000000000000, -1.000000000000000000 ) ) ;
#11801 = ADVANCED_FACE ( 'NONE', ( #2802 ), #6737, .F. ) ;
#11802 = VERTEX_POINT ( 'NONE', #295 ) ;
#11803 = ORIENTED_EDGE ( 'NONE', *, *, #10389, .F. ) ;
#11804 = AXIS2_PLACEMENT_3D ( 'NONE', #6933, #11300, #1411 ) ;
#11805 = CARTESIAN_POINT ( 'NONE',  ( 0.000000000000000000, 5.051668046482832750E-16, -4.000000000000000000 ) ) ;
#11806 = PRODUCT_DEFINITION_SHAPE ( 'NONE', 'NONE',  #14370 ) ;
#11807 = CARTESIAN_POINT ( 'NONE',  ( 0.06760930072668812352, 0.5150000000000032330, -0.9010842325122888630 ) ) ;
#11808 = ORIENTED_EDGE ( 'NONE', *, *, #4120, .T. ) ;
#11809 = CARTESIAN_POINT ( 'NONE',  ( 0.000000000000000000, 0.000000000000000000, 200.0000000000000000 ) ) ;
#11810 = EDGE_CURVE ( 'NONE', #12491, #5369, #4896, .T. ) ;
#11811 = EDGE_CURVE ( 'NONE', #3034, #3774, #5817, .T. ) ;
#11812 = LINE ( 'NONE', #92, #12927 ) ;
#11813 = CIRCLE ( 'NONE', #1105, 0.2000000000000022593 ) ;
#11814 = FACE_OUTER_BOUND ( 'NONE', #7449, .T. ) ;
#11815 = DIRECTION ( 'NONE',  ( 0.000000000000000000, 1.224646799147353207E-16, 1.000000000000000000 ) ) ;
#11816 = VECTOR ( 'NONE', #5069, 1000.000000000000000 ) ;
#11817 = ADVANCED_FACE ( 'NONE', ( #13743 ), #9109, .F. ) ;
#11818 = CONTEXT_DEPENDENT_SHAPE_REPRESENTATION ( #4752, #1838 ) ;
#11819 = VECTOR ( 'NONE', #9011, 1000.000000000000000 ) ;
#11820 = VERTEX_POINT ( 'NONE', #12650 ) ;
#11821 = PLANE ( 'NONE',  #10793 ) ;
#11822 = EDGE_LOOP ( 'NONE', ( #2039, #1028 ) ) ;
#11823 = DIRECTION ( 'NONE',  ( -1.000000000000000000, -0.000000000000000000, -0.000000000000000000 ) ) ;
#11824 = CARTESIAN_POINT ( 'NONE',  ( 2.500000000000000000, -1.768423874527823791, -1.020999999999998353 ) ) ;
#11825 = AXIS2_PLACEMENT_3D ( 'NONE', #6580, #7450, #11880 ) ;
#11826 = ORIENTED_EDGE ( 'NONE', *, *, #12000, .F. ) ;
#11827 = DIRECTION ( 'NONE',  ( -1.000000000000000000, 0.000000000000000000, 0.000000000000000000 ) ) ;
#11828 = ORIENTED_EDGE ( 'NONE', *, *, #11262, .T. ) ;
#11829 = PLANE ( 'NONE',  #2698 ) ;
#11830 = EDGE_CURVE ( 'NONE', #12612, #246, #8593, .T. ) ;
#11831 = CARTESIAN_POINT ( 'NONE',  ( -4.211140560182196957, -2.431303136016552013, -3.745885042887436178 ) ) ;
#11832 = EDGE_LOOP ( 'NONE', ( #805, #4465, #10426 ) ) ;
#11833 = CARTESIAN_POINT ( 'NONE',  ( 299.9999999999999432, -95.00000000000008527, -186.2999999999999829 ) ) ;
#11834 = EDGE_CURVE ( 'NONE', #1900, #6925, #9173, .T. ) ;
#11835 = AXIS2_PLACEMENT_3D ( 'NONE', #7722, #4538, #3523 ) ;
#11836 = CARTESIAN_POINT ( 'NONE',  ( 53.33333333333330017, -25.00000000000000000, -222.5000000000000853 ) ) ;
#11837 = FILL_AREA_STYLE ('',( #4071 ) ) ;
#11838 =( NAMED_UNIT ( * ) SI_UNIT ( $, .STERADIAN. ) SOLID_ANGLE_UNIT ( ) );
#11839 = EDGE_CURVE ( 'NONE', #5456, #532, #13085, .T. ) ;
#11840 = CONTEXT_DEPENDENT_SHAPE_REPRESENTATION ( #2660, #10009 ) ;
#11841 = CARTESIAN_POINT ( 'NONE',  ( 0.000000000000000000, 0.000000000000000000, 0.000000000000000000 ) ) ;
#11842 = AXIS2_PLACEMENT_3D ( 'NONE', #12888, #13974, #7451 ) ;
#11843 = ORIENTED_EDGE ( 'NONE', *, *, #14163, .T. ) ;
#11844 = ORIENTED_EDGE ( 'NONE', *, *, #340, .F. ) ;
#11845 = FACE_BOUND ( 'NONE', #2059, .T. ) ;
#11846 =( REPRESENTATION_RELATIONSHIP ('NONE','NONE', #11251, #9307 ) REPRESENTATION_RELATIONSHIP_WITH_TRANSFORMATION ( #6249 )SHAPE_REPRESENTATION_RELATIONSHIP( ) );
#11847 = ORIENTED_EDGE ( 'NONE', *, *, #12224, .F. ) ;
#11848 = CIRCLE ( 'NONE', #7659, 4.250000000000000000 ) ;
#11849 = CARTESIAN_POINT ( 'NONE',  ( 2.000000000000005329, -3.464101615137751722, 0.000000000000000000 ) ) ;
#11850 = ORIENTED_EDGE ( 'NONE', *, *, #9850, .T. ) ;
#11851 = ORIENTED_EDGE ( 'NONE', *, *, #8018, .T. ) ;
#11852 = DIRECTION ( 'NONE',  ( 0.000000000000000000, 1.000000000000000000, 0.000000000000000000 ) ) ;
#11853 = ORIENTED_EDGE ( 'NONE', *, *, #6816, .F. ) ;
#11854 = DIRECTION ( 'NONE',  ( 1.000000000000000000, 0.000000000000000000, 0.000000000000000000 ) ) ;
#11855 = UNCERTAINTY_MEASURE_WITH_UNIT (LENGTH_MEASURE( 1.000000000000000082E-05 ), #852, 'distance_accuracy_value', 'NONE');
#11856 = DIRECTION ( 'NONE',  ( -0.000000000000000000, -0.000000000000000000, -1.000000000000000000 ) ) ;
#11857 = VECTOR ( 'NONE', #6786, 1000.000000000000000 ) ;
#11858 = FACE_OUTER_BOUND ( 'NONE', #3362, .T. ) ;
#11859 = DIRECTION ( 'NONE',  ( -0.000000000000000000, 0.000000000000000000, -1.000000000000000000 ) ) ;
#11860 = DIRECTION ( 'NONE',  ( -1.000000000000000000, 0.000000000000000000, 0.000000000000000000 ) ) ;
#11861 = EDGE_LOOP ( 'NONE', ( #12059, #3922 ) ) ;
#11862 = EDGE_LOOP ( 'NONE', ( #11132, #4083, #6738, #4441 ) ) ;
#11863 = TOROIDAL_SURFACE ( 'NONE', #14, 4.000000000000000000, 0.2500000000000000000 ) ;
#11864 = ADVANCED_FACE ( 'NONE', ( #12013 ), #12872, .F. ) ;
#11865 = DIRECTION ( 'NONE',  ( 0.000000000000000000, 0.000000000000000000, 1.000000000000000000 ) ) ;
#11866 = AXIS2_PLACEMENT_3D ( 'NONE', #1121, #14196, #2378 ) ;
#11867 = LINE ( 'NONE', #7436, #7560 ) ;
#11868 = DIRECTION ( 'NONE',  ( 0.000000000000000000, -1.000000000000000000, 1.287488025362403787E-15 ) ) ;
#11869 = FACE_BOUND ( 'NONE', #5185, .T. ) ;
#11870 = ORIENTED_EDGE ( 'NONE', *, *, #1056, .T. ) ;
#11871 = AXIS2_PLACEMENT_3D ( 'NONE', #542, #11524, #12751 ) ;
#11872 = FACE_OUTER_BOUND ( 'NONE', #8166, .T. ) ;
#11873 = AXIS2_PLACEMENT_3D ( 'NONE', #1928, #2809, #7225 ) ;
#11874 = LINE ( 'NONE', #4184, #12505 ) ;
#11875 = CARTESIAN_POINT ( 'NONE',  ( 2.220446049250313081E-13, 90.00000000000001421, 129.9999999999999716 ) ) ;
#11876 = DIRECTION ( 'NONE',  ( -0.000000000000000000, -0.000000000000000000, 1.000000000000000000 ) ) ;
#11877 = VECTOR ( 'NONE', #4446, 1000.000000000000000 ) ;
#11878 = EDGE_LOOP ( 'NONE', ( #1658, #11570, #6957, #9532 ) ) ;
#11879 = ORIENTED_EDGE ( 'NONE', *, *, #12593, .T. ) ;
#11880 = DIRECTION ( 'NONE',  ( 0.000000000000000000, 0.000000000000000000, -1.000000000000000000 ) ) ;
#11882 = CIRCLE ( 'NONE', #1202, 2.649999999999985700 ) ;
#11881 = VECTOR ( 'NONE', #12945, 1000.000000000000000 ) ;
#11883 = DIRECTION ( 'NONE',  ( -1.000000000000000000, -0.000000000000000000, -0.000000000000000000 ) ) ;
#11884 = CARTESIAN_POINT ( 'NONE',  ( 0.3461262719736147297, -4.658553426539303821, -3.671615880910379381 ) ) ;
#11885 = PRODUCT_DEFINITION_CONTEXT ( 'detailed design', #1924, 'design' ) ;
#11886 = PRESENTATION_LAYER_ASSIGNMENT (  '', '', ( #7009 ) ) ;
#11887 = VERTEX_POINT ( 'NONE', #4252 ) ;
#11889 = ADVANCED_FACE ( 'NONE', ( #3101 ), #2063, .F. ) ;
#11888 = CARTESIAN_POINT ( 'NONE',  ( 53.33333333333330017, -25.00000000000000000, 219.8500000000001080 ) ) ;
#11890 = EDGE_CURVE ( 'NONE', #14065, #2517, #2876, .T. ) ;
#11891 = LINE ( 'NONE', #10802, #8524 ) ;
#11892 = DIRECTION ( 'NONE',  ( 0.000000000000000000, 0.000000000000000000, 1.000000000000000000 ) ) ;
#11893 = LINE ( 'NONE', #12974, #13392 ) ;
#11894 = AXIS2_PLACEMENT_3D ( 'NONE', #5304, #697, #8475 ) ;
#11895 = ITEM_DEFINED_TRANSFORMATION ( 'NONE', 'NONE', #10483,  #14039 ) ;
#11896 = EDGE_LOOP ( 'NONE', ( #9432, #10704, #11468, #10828, #9932 ) ) ;
#11897 = CARTESIAN_POINT ( 'NONE',  ( 219.9999999999999716, -14.99999999999999822, 219.8500000000001080 ) ) ;
#11898 = ORIENTED_EDGE ( 'NONE', *, *, #6587, .T. ) ;
#11899 = LINE ( 'NONE', #1945, #9521 ) ;
#11900 = CARTESIAN_POINT ( 'NONE',  ( 137.6499999999999488, -56.99999999999997158, 0.000000000000000000 ) ) ;
#11901 = ORIENTED_EDGE ( 'NONE', *, *, #11218, .F. ) ;
#11902 = CARTESIAN_POINT ( 'NONE',  ( 303.3333333333333144, -14.99999999999999822, 222.5000000000000853 ) ) ;
#11903 = ORIENTED_EDGE ( 'NONE', *, *, #4277, .F. ) ;
#11905 = EDGE_CURVE ( 'NONE', #12712, #7175, #3168, .T. ) ;
#11904 = DIRECTION ( 'NONE',  ( -0.000000000000000000, 1.000000000000000000, -0.000000000000000000 ) ) ;
#11906 = EDGE_CURVE ( 'NONE', #9162, #11555, #9664, .T. ) ;
#11907 = CARTESIAN_POINT ( 'NONE',  ( -299.9999999999999432, -75.00000000000008527, 339.9999999999999432 ) ) ;
#11908 = ORIENTED_EDGE ( 'NONE', *, *, #7024, .F. ) ;
#11909 = CARTESIAN_POINT ( 'NONE',  ( 17.00000000000000000, 0.000000000000000000, 0.000000000000000000 ) ) ;
#11910 = CARTESIAN_POINT ( 'NONE',  ( 386.6666666666666288, -25.00000000000000000, -222.5000000000000853 ) ) ;
#11911 = EDGE_CURVE ( 'NONE', #7429, #1850, #14271, .T. ) ;
#11912 = CARTESIAN_POINT ( 'NONE',  ( 2.500000000000000000, -1.178949249685214307, 2.042000000000001592 ) ) ;
#11913 = CONTEXT_DEPENDENT_SHAPE_REPRESENTATION ( #6375, #3569 ) ;
#11914 = CARTESIAN_POINT ( 'NONE',  ( -3.999999999998910649, -1.658469974638591804, -3.531532913075256186 ) ) ;
#11915 = ORIENTED_EDGE ( 'NONE', *, *, #11289, .T. ) ;
#11916 = VERTEX_POINT ( 'NONE', #6423 ) ;
#11917 = EDGE_CURVE ( 'NONE', #3111, #1839, #11507, .T. ) ;
#11918 = ADVANCED_FACE ( 'NONE', ( #4175 ), #881, .F. ) ;
#11919 = CARTESIAN_POINT ( 'NONE',  ( 136.6666666666666288, -15.00000000000000000, 225.1500000000000625 ) ) ;
#11920 = VERTEX_POINT ( 'NONE', #9765 ) ;
#11921 = ADVANCED_FACE ( 'NONE', ( #14101 ), #12649, .T. ) ;
#11922 = EDGE_CURVE ( 'NONE', #4821, #4081, #590, .T. ) ;
#11923 = DIRECTION ( 'NONE',  ( 0.000000000000000000, 0.000000000000000000, -1.000000000000000000 ) ) ;
#11924 = UNCERTAINTY_MEASURE_WITH_UNIT (LENGTH_MEASURE( 1.000000000000000082E-05 ), #8462, 'distance_accuracy_value', 'NONE');
#11925 = ORIENTED_EDGE ( 'NONE', *, *, #4301, .F. ) ;
#11926 = VERTEX_POINT ( 'NONE', #10711 ) ;
#11927 = DIRECTION ( 'NONE',  ( -7.304098846218135653E-17, 1.000000000000000000, 0.000000000000000000 ) ) ;
#11928 = ORIENTED_EDGE ( 'NONE', *, *, #188, .T. ) ;
#11929 = PLANE ( 'NONE',  #7543 ) ;
#11930 = EDGE_CURVE ( 'NONE', #6823, #682, #11867, .T. ) ;
#11931 = LINE ( 'NONE', #6408, #13593 ) ;
#11932 = LINE ( 'NONE', #938, #11064 ) ;
#11933 = SURFACE_STYLE_FILL_AREA ( #6265 ) ;
#11934 = PLANE ( 'NONE',  #4581 ) ;
#11935 = ORIENTED_EDGE ( 'NONE', *, *, #1177, .T. ) ;
#11936 = VERTEX_POINT ( 'NONE', #740 ) ;
#11937 = CARTESIAN_POINT ( 'NONE',  ( -222.6499999999998920, -85.00000000000009948, 40.00000000000000000 ) ) ;
#11938 = VERTEX_POINT ( 'NONE', #1766 ) ;
#11939 = DIRECTION ( 'NONE',  ( -0.000000000000000000, 1.000000000000000000, -0.000000000000000000 ) ) ;
#11940 = CARTESIAN_POINT ( 'NONE',  ( 1.849560077140108172, -0.7556913915602447851, 0.5149999999999994582 ) ) ;
#11941 = VECTOR ( 'NONE', #10230, 1000.000000000000000 ) ;
#11942 = FACE_BOUND ( 'NONE', #2057, .T. ) ;
#11943 = CIRCLE ( 'NONE', #10549, 5.500000000000005329 ) ;
#11944 = ORIENTED_EDGE ( 'NONE', *, *, #11839, .F. ) ;
#11945 = DIRECTION ( 'NONE',  ( -1.000000000000000000, 0.000000000000000000, 0.000000000000000000 ) ) ;
#11946 = EDGE_CURVE ( 'NONE', #1416, #9015, #10636, .T. ) ;
#11947 = CARTESIAN_POINT ( 'NONE',  ( 8.000000000000000000, -4.837354856632045452E-15, 0.000000000000000000 ) ) ;
#11948 = CARTESIAN_POINT ( 'NONE',  ( 236.4999999999999432, -85.00000000000007105, 200.0000000000000000 ) ) ;
#11949 = DIRECTION ( 'NONE',  ( 0.000000000000000000, 0.000000000000000000, -1.000000000000000000 ) ) ;
#11950 = ORIENTED_EDGE ( 'NONE', *, *, #12706, .F. ) ;
#11951 = AXIS2_PLACEMENT_3D ( 'NONE', #4867, #9287, #7169 ) ;
#11952 = VERTEX_POINT ( 'NONE', #5132 ) ;
#11953 = CARTESIAN_POINT ( 'NONE',  ( 0.000000000000000000, 0.000000000000000000, -5.000000000000000000 ) ) ;
#11954 = CARTESIAN_POINT ( 'NONE',  ( 1.849560077140107284, 0.5150000000000026779, -0.7556913915602427867 ) ) ;
#11955 = ORIENTED_EDGE ( 'NONE', *, *, #3697, .F. ) ;
#11956 = CYLINDRICAL_SURFACE ( 'NONE', #6642, 2.649999999999985700 ) ;
#11957 = AXIS2_PLACEMENT_3D ( 'NONE', #12935, #14156, #4238 ) ;
#11958 = CARTESIAN_POINT ( 'NONE',  ( 134.9999999999999432, -56.99999999999997158, -169.9999999999999716 ) ) ;
#11959 = DIRECTION ( 'NONE',  ( -0.5000000000000051070, 0.000000000000000000, 0.8660254037844355990 ) ) ;
#11960 = CONTEXT_DEPENDENT_SHAPE_REPRESENTATION ( #10961, #3804 ) ;
#11961 = EDGE_LOOP ( 'NONE', ( #11284, #10538, #13777, #11482 ) ) ;
#11962 = EDGE_CURVE ( 'NONE', #3954, #11114, #4550, .T. ) ;
#11963 = CARTESIAN_POINT ( 'NONE',  ( -30.00000000000002842, -225.0000000000000000, -190.0000000000000000 ) ) ;
#11964 = AXIS2_PLACEMENT_3D ( 'NONE', #2820, #10354, #2747 ) ;
#11965 = VERTEX_POINT ( 'NONE', #1921 ) ;
#11966 = CARTESIAN_POINT ( 'NONE',  ( 0.000000000000000000, 0.000000000000000000, 3.469446951953614189E-15 ) ) ;
#11967 = DIRECTION ( 'NONE',  ( 0.000000000000000000, -0.000000000000000000, -1.000000000000000000 ) ) ;
#11968 = AXIS2_PLACEMENT_3D ( 'NONE', #2421, #2282, #8813 ) ;
#11969 = ORIENTED_EDGE ( 'NONE', *, *, #12339, .T. ) ;
#11970 = ORIENTED_EDGE ( 'NONE', *, *, #5693, .F. ) ;
#11971 = CARTESIAN_POINT ( 'NONE',  ( 1.799999999999996048, 0.000000000000000000, -9.999999999999994671 ) ) ;
#11972 = DIRECTION ( 'NONE',  ( -0.000000000000000000, 1.000000000000000000, -0.000000000000000000 ) ) ;
#11973 = VERTEX_POINT ( 'NONE', #8595 ) ;
#11974 = AXIS2_PLACEMENT_3D ( 'NONE', #12526, #4848, #2593 ) ;
#11975 = SURFACE_STYLE_FILL_AREA ( #8705 ) ;
#11976 = AXIS2_PLACEMENT_3D ( 'NONE', #11364, #9181, #8087 ) ;
#11977 = FACE_OUTER_BOUND ( 'NONE', #5192, .T. ) ;
#11978 = VECTOR ( 'NONE', #12579, 1000.000000000000000 ) ;
#11979 =( NAMED_UNIT ( * ) SI_UNIT ( $, .STERADIAN. ) SOLID_ANGLE_UNIT ( ) );
#11980 = CARTESIAN_POINT ( 'NONE',  ( -25.39999999999996305, 5.817072295949926440E-16, -4.749999999999999112 ) ) ;
#11981 = CONTEXT_DEPENDENT_SHAPE_REPRESENTATION ( #5820, #10278 ) ;
#11982 = CIRCLE ( 'NONE', #6188, 12.77499999999999858 ) ;
#11983 = FACE_OUTER_BOUND ( 'NONE', #4656, .T. ) ;
#11984 = ORIENTED_EDGE ( 'NONE', *, *, #5091, .F. ) ;
#11985 = ORIENTED_EDGE ( 'NONE', *, *, #5065, .T. ) ;
#11986 = EDGE_CURVE ( 'NONE', #1982, #7287, #2942, .T. ) ;
#11987 = DIRECTION ( 'NONE',  ( 0.000000000000000000, 1.000000000000000000, 1.224646799147353207E-16 ) ) ;
#11988 = ORIENTED_EDGE ( 'NONE', *, *, #11387, .F. ) ;
#11989 = CARTESIAN_POINT ( 'NONE',  ( -4.000000000000003553, 2.309401076758496263, -3.504269196027868905 ) ) ;
#11990 = VERTEX_POINT ( 'NONE', #5271 ) ;
#11991 = CIRCLE ( 'NONE', #13587, 2.649999999999985700 ) ;
#11992 = ORIENTED_EDGE ( 'NONE', *, *, #3564, .F. ) ;
#11993 = DIRECTION ( 'NONE',  ( -1.000000000000000000, 0.000000000000000000, 0.000000000000000000 ) ) ;
#11994 = ORIENTED_EDGE ( 'NONE', *, *, #434, .F. ) ;
#11995 = LINE ( 'NONE', #8505, #10801 ) ;
#11996 = AXIS2_PLACEMENT_3D ( 'NONE', #267, #1447, #9217 ) ;
#11997 = AXIS2_PLACEMENT_3D ( 'NONE', #10378, #6025, #9145 ) ;
#11998 = DIRECTION ( 'NONE',  ( -1.000000000000000000, 0.000000000000000000, 0.000000000000000000 ) ) ;
#11999 = LINE ( 'NONE', #5257, #4801 ) ;
#12000 = EDGE_CURVE ( 'NONE', #9004, #140, #1998, .T. ) ;
#12001 = ADVANCED_FACE ( 'NONE', ( #8740 ), #1101, .F. ) ;
#12002 = CARTESIAN_POINT ( 'NONE',  ( -135.0000000000000000, -95.00000000000008527, 30.00000000000000000 ) ) ;
#12003 = VECTOR ( 'NONE', #9012, 1000.000000000000000 ) ;
#12004 = EDGE_CURVE ( 'NONE', #4187, #5968, #7100, .T. ) ;
#12005 = DIRECTION ( 'NONE',  ( 1.000000000000000000, 0.000000000000000000, 0.000000000000000000 ) ) ;
#12006 = CONICAL_SURFACE ( 'NONE', #14069, 2.500000000000002220, 1.029744260000002631 ) ;
#12007 = DIRECTION ( 'NONE',  ( 0.000000000000000000, 1.000000000000000000, 0.000000000000000000 ) ) ;
#12008 = EDGE_LOOP ( 'NONE', ( #8281, #7236 ) ) ;
#12009 = CIRCLE ( 'NONE', #13264, 2.649999999999985700 ) ;
#12010 = EDGE_LOOP ( 'NONE', ( #12192, #13157, #10527, #4578 ) ) ;
#12011 = LINE ( 'NONE', #6776, #4484 ) ;
#12012 = ORIENTED_EDGE ( 'NONE', *, *, #8150, .F. ) ;
#12013 = FACE_OUTER_BOUND ( 'NONE', #4763, .T. ) ;
#12014 = CARTESIAN_POINT ( 'NONE',  ( 0.000000000000000000, 1.178949249685213863, -2.042000000000001148 ) ) ;
#12015 =( NAMED_UNIT ( * ) SI_UNIT ( $, .STERADIAN. ) SOLID_ANGLE_UNIT ( ) );
#12016 = ORIENTED_EDGE ( 'NONE', *, *, #747, .F. ) ;
#12017 = VECTOR ( 'NONE', #6261, 1000.000000000000000 ) ;
#12018 = EDGE_CURVE ( 'NONE', #11113, #13081, #3627, .T. ) ;
#12019 = DIRECTION ( 'NONE',  ( -0.000000000000000000, -0.000000000000000000, 1.000000000000000000 ) ) ;
#12020 = CARTESIAN_POINT ( 'NONE',  ( 2.740000000000000213, 0.9838866223910003317, 0.5149999999999999023 ) ) ;
#12021 = DIRECTION ( 'NONE',  ( 6.123233995736766036E-17, 0.000000000000000000, -1.000000000000000000 ) ) ;
#12022 = DIRECTION ( 'NONE',  ( -0.000000000000000000, -1.000000000000000000, -0.000000000000000000 ) ) ;
#12023 = EDGE_LOOP ( 'NONE', ( #8437, #1828 ) ) ;
#12024 = ORIENTED_EDGE ( 'NONE', *, *, #3787, .T. ) ;
#12025 = CARTESIAN_POINT ( 'NONE',  ( 0.000000000000000000, -2.357898499370432610, 3.252606517456513302E-15 ) ) ;
#12026 = CARTESIAN_POINT ( 'NONE',  ( 5.000000000000000888, 0.000000000000000000, 0.000000000000000000 ) ) ;
#12027 = CONICAL_SURFACE ( 'NONE', #4608, 2.500000000000000888, 0.9599310885968785900 ) ;
#12028 = ORIENTED_EDGE ( 'NONE', *, *, #894, .T. ) ;
#12029 = PLANE ( 'NONE',  #125 ) ;
#12030 = CARTESIAN_POINT ( 'NONE',  ( 299.9999999999999432, -75.00000000000008527, -190.0000000000000000 ) ) ;
#12031 = CARTESIAN_POINT ( 'NONE',  ( 470.0000000000000000, -20.00000000000000000, 200.0000000000000000 ) ) ;
#12032 = DIRECTION ( 'NONE',  ( -1.000000000000000000, 0.000000000000000000, 0.000000000000000000 ) ) ;
#12033 = APPLICATION_CONTEXT ( 'automotive_design' ) ;
#12034 = AXIS2_PLACEMENT_3D ( 'NONE', #599, #7293, #3107 ) ;
#12035 = ORIENTED_EDGE ( 'NONE', *, *, #8445, .T. ) ;
#12036 = FACE_OUTER_BOUND ( 'NONE', #647, .T. ) ;
#12037 = ORIENTED_EDGE ( 'NONE', *, *, #9646, .F. ) ;
#12038 = EDGE_CURVE ( 'NONE', #5337, #8377, #1024, .T. ) ;
#12039 = CARTESIAN_POINT ( 'NONE',  ( 2.500000000000000888, 3.061616997868384127E-16, -4.974599999999998801 ) ) ;
#12040 = CARTESIAN_POINT ( 'NONE',  ( -304.9999999999999432, -95.00000000000008527, 30.00000000000002842 ) ) ;
#12041 = VERTEX_POINT ( 'NONE', #8950 ) ;
#12042 = VERTEX_POINT ( 'NONE', #2205 ) ;
#12043 = CIRCLE ( 'NONE', #3935, 13.50000000000000000 ) ;
#12044 = DIRECTION ( 'NONE',  ( 1.000000000000000000, 0.000000000000000000, 0.000000000000000000 ) ) ;
#12045 = UNCERTAINTY_MEASURE_WITH_UNIT (LENGTH_MEASURE( 1.000000000000000082E-05 ), #1891, 'distance_accuracy_value', 'NONE');
#12046 = PRODUCT_DEFINITION_SHAPE ( 'NONE', 'NONE',  #14356 ) ;
#12047 = CARTESIAN_POINT ( 'NONE',  ( 5.200000000000002842, 3.306546357697854226E-16, 2.700000000000000622 ) ) ;
#12048 = EDGE_LOOP ( 'NONE', ( #3035, #5806, #5500 ) ) ;
#12049 = AXIS2_PLACEMENT_3D ( 'NONE', #11162, #33, #3543 ) ;
#12050 = CARTESIAN_POINT ( 'NONE',  ( -314.9999999999999432, -105.0000000000000995, 30.00000000000000000 ) ) ;
#12051 = VECTOR ( 'NONE', #2149, 1000.000000000000000 ) ;
#12052 = CARTESIAN_POINT ( 'NONE',  ( -20.63749999999999929, 0.000000000000000000, 0.000000000000000000 ) ) ;
#12053 = CARTESIAN_POINT ( 'NONE',  ( 470.0000000000000000, -20.00000000000000000, 240.0000000000000284 ) ) ;
#12054 = CYLINDRICAL_SURFACE ( 'NONE', #11502, 10.00000000000000000 ) ;
#12055 =( NAMED_UNIT ( * ) SI_UNIT ( $, .STERADIAN. ) SOLID_ANGLE_UNIT ( ) );
#12056 = CARTESIAN_POINT ( 'NONE',  ( 434.9999999999999432, 8.660254037844390851, 205.0000000000000284 ) ) ;
#12057 = CARTESIAN_POINT ( 'NONE',  ( -299.9999999999999432, -75.00000000000008527, 39.99999999999997868 ) ) ;
#12058 = ORIENTED_EDGE ( 'NONE', *, *, #1878, .F. ) ;
#12059 = ORIENTED_EDGE ( 'NONE', *, *, #14032, .F. ) ;
#12060 = LINE ( 'NONE', #4443, #9378 ) ;
#12061 = VERTEX_POINT ( 'NONE', #13367 ) ;
#12062 = CARTESIAN_POINT ( 'NONE',  ( 386.6666666666666288, -25.00000000000000000, -219.8500000000001080 ) ) ;
#12063 = VERTEX_POINT ( 'NONE', #7779 ) ;
#12064 = VERTEX_POINT ( 'NONE', #12216 ) ;
#12065 = CARTESIAN_POINT ( 'NONE',  ( -20.00000000000000000, 0.000000000000000000, 190.0000000000000000 ) ) ;
#12066 = ORIENTED_EDGE ( 'NONE', *, *, #9992, .F. ) ;
#12067 = CIRCLE ( 'NONE', #9044, 7.864440107515625833 ) ;
#12068 = CARTESIAN_POINT ( 'NONE',  ( 2.500000000000000000, 0.000000000000000000, 0.000000000000000000 ) ) ;
#12069 = PLANE ( 'NONE',  #7118 ) ;
#12070 = DIRECTION ( 'NONE',  ( -0.000000000000000000, -0.000000000000000000, 1.000000000000000000 ) ) ;
#12071 = EDGE_CURVE ( 'NONE', #7265, #8495, #8952, .T. ) ;
#12072 = DIRECTION ( 'NONE',  ( 1.000000000000000000, 0.000000000000000000, 0.000000000000000000 ) ) ;
#12073 = EDGE_CURVE ( 'NONE', #2710, #2006, #2923, .T. ) ;
#12074 = LINE ( 'NONE', #14161, #9908 ) ;
#12075 = ORIENTED_EDGE ( 'NONE', *, *, #11764, .T. ) ;
#12076 = ORIENTED_EDGE ( 'NONE', *, *, #13560, .F. ) ;
#12077 = ADVANCED_FACE ( 'NONE', ( #5622 ), #13237, .F. ) ;
#12078 = DIRECTION ( 'NONE',  ( -1.000000000000000000, -0.000000000000000000, -0.000000000000000000 ) ) ;
#12079 = AXIS2_PLACEMENT_3D ( 'NONE', #1546, #9329, #5912 ) ;
#12080 = ORIENTED_EDGE ( 'NONE', *, *, #10302, .F. ) ;
#12081 = CARTESIAN_POINT ( 'NONE',  ( -3.679171394226034675, -2.494631558665844739, -0.3503314178412558211 ) ) ;
#12082 = LINE ( 'NONE', #5, #10259 ) ;
#12083 = CARTESIAN_POINT ( 'NONE',  ( -124.9999999999999432, 55.00000000000001421, 40.00000000000000000 ) ) ;
#12084 = EDGE_LOOP ( 'NONE', ( #5546, #10850, #11471, #13973, #12479 ) ) ;
#12085 = EDGE_CURVE ( 'NONE', #4114, #3377, #4532, .T. ) ;
#12086 = CARTESIAN_POINT ( 'NONE',  ( 219.9999999999999716, -20.00000000000000000, 225.1500000000000625 ) ) ;
#12087 = LINE ( 'NONE', #4324, #3674 ) ;
#12088 = VECTOR ( 'NONE', #13734, 1000.000000000000000 ) ;
#12089 = DIRECTION ( 'NONE',  ( 0.000000000000000000, 0.000000000000000000, -1.000000000000000000 ) ) ;
#12090 = ORIENTED_EDGE ( 'NONE', *, *, #11930, .T. ) ;
#12091 = ORIENTED_EDGE ( 'NONE', *, *, #10565, .F. ) ;
#12092 = EDGE_CURVE ( 'NONE', #11346, #1964, #2138, .T. ) ;
#12093 = CARTESIAN_POINT ( 'NONE',  ( -10.00000000000000000, 0.000000000000000000, -200.0000000000000000 ) ) ;
#12094 = EDGE_CURVE ( 'NONE', #2563, #11122, #832, .T. ) ;
#12095 = PLANE ( 'NONE',  #7200 ) ;
#12096 = ORIENTED_EDGE ( 'NONE', *, *, #14198, .T. ) ;
#12097 = DIRECTION ( 'NONE',  ( 1.000000000000000000, 0.000000000000000000, 0.000000000000000000 ) ) ;
#12098 = EDGE_CURVE ( 'NONE', #12042, #6338, #11056, .T. ) ;
#12099 = CARTESIAN_POINT ( 'NONE',  ( 124.9999999999999574, -64.99999999999997158, 0.000000000000000000 ) ) ;
#12100 = CIRCLE ( 'NONE', #2376, 5.500000000000005329 ) ;
#12101 = CARTESIAN_POINT ( 'NONE',  ( 119.9999999999999147, -24.99999999999999289, 19.99999999999998934 ) ) ;
#12102 = CARTESIAN_POINT ( 'NONE',  ( 0.000000000000000000, 0.000000000000000000, -188.0000000000000000 ) ) ;
#12103 = VECTOR ( 'NONE', #1700, 1000.000000000000000 ) ;
#12104 = ORIENTED_EDGE ( 'NONE', *, *, #11834, .T. ) ;
#12105 = CARTESIAN_POINT ( 'NONE',  ( 469.9999999999998863, -225.0000000000000000, 190.0000000000000000 ) ) ;
#12106 = PRODUCT_DEFINITION_FORMATION_WITH_SPECIFIED_SOURCE ( 'ANY', '', #2407, .NOT_KNOWN. ) ;
#12107 =( GEOMETRIC_REPRESENTATION_CONTEXT ( 3 ) GLOBAL_UNCERTAINTY_ASSIGNED_CONTEXT ( ( #2041 ) ) GLOBAL_UNIT_ASSIGNED_CONTEXT ( ( #8000, #7002, #5910 ) ) REPRESENTATION_CONTEXT ( 'NONE', 'WORKASPACE' ) );
#12108 = VERTEX_POINT ( 'NONE', #1247 ) ;
#12109 = AXIS2_PLACEMENT_3D ( 'NONE', #1294, #11396, #3432 ) ;
#12110 = CARTESIAN_POINT ( 'NONE',  ( 140.0000000000000000, -95.00000000000008527, 190.0000000000000000 ) ) ;
#12111 = CARTESIAN_POINT ( 'NONE',  ( 0.000000000000000000, 1.178949249685218525, 2.041999999999999371 ) ) ;
#12112 = ORIENTED_EDGE ( 'NONE', *, *, #14237, .T. ) ;
#12113 = VERTEX_POINT ( 'NONE', #13438 ) ;
#12114 = CARTESIAN_POINT ( 'NONE',  ( 140.0000000000000000, -95.00000000000008527, 186.2999999999999829 ) ) ;
#12115 = CARTESIAN_POINT ( 'NONE',  ( -30.00000000000002842, -20.00000000000000000, -250.0000000000000000 ) ) ;
#12116 = DIRECTION ( 'NONE',  ( -0.000000000000000000, 0.000000000000000000, -1.000000000000000000 ) ) ;
#12117 = CARTESIAN_POINT ( 'NONE',  ( 136.6666666666666288, -20.00000000000000000, -222.5000000000000853 ) ) ;
#12118 = CARTESIAN_POINT ( 'NONE',  ( -2.000000000000007550, -3.464101615137749945, 0.000000000000000000 ) ) ;
#12119 = CYLINDRICAL_SURFACE ( 'NONE', #6537, 2.649999999999985700 ) ;
#12120 = DIRECTION ( 'NONE',  ( -0.000000000000000000, -0.000000000000000000, 1.000000000000000000 ) ) ;
#12121 = EDGE_CURVE ( 'NONE', #13122, #9002, #2237, .T. ) ;
#12122 = DIRECTION ( 'NONE',  ( -1.000000000000000000, 0.000000000000000000, 0.000000000000000000 ) ) ;
#12123 = CYLINDRICAL_SURFACE ( 'NONE', #6892, 2.500000000000002220 ) ;
#12124 = ORIENTED_EDGE ( 'NONE', *, *, #74, .F. ) ;
#12125 = ORIENTED_EDGE ( 'NONE', *, *, #6889, .F. ) ;
#12126 = DIRECTION ( 'NONE',  ( -0.000000000000000000, 1.000000000000000000, -0.000000000000000000 ) ) ;
#12127 = ORIENTED_EDGE ( 'NONE', *, *, #2035, .T. ) ;
#12128 = LINE ( 'NONE', #7489, #7465 ) ;
#12129 = EDGE_LOOP ( 'NONE', ( #4422, #12569, #9621, #1472 ) ) ;
#12130 = ORIENTED_EDGE ( 'NONE', *, *, #4200, .F. ) ;
#12131 = CARTESIAN_POINT ( 'NONE',  ( -0.2277608394786177770, 0.000000000000000000, 0.000000000000000000 ) ) ;
#12132 = ORIENTED_EDGE ( 'NONE', *, *, #12195, .F. ) ;
#12133 = DIRECTION ( 'NONE',  ( -1.000000000000000000, 0.000000000000000000, -0.000000000000000000 ) ) ;
#12134 = DIRECTION ( 'NONE',  ( 0.000000000000000000, -1.224646799147353454E-16, 1.000000000000000000 ) ) ;
#12135 = DIRECTION ( 'NONE',  ( 0.000000000000000000, -3.491481338843133355E-15, 1.000000000000000000 ) ) ;
#12136 = CARTESIAN_POINT ( 'NONE',  ( 219.9999999999999716, -85.00000000000007105, -250.0009999999999764 ) ) ;
#12137 = DIRECTION ( 'NONE',  ( 0.000000000000000000, -0.5000000000000013323, -0.8660254037844380415 ) ) ;
#12138 = DIRECTION ( 'NONE',  ( -0.000000000000000000, -0.000000000000000000, -1.000000000000000000 ) ) ;
#12139 = ORIENTED_EDGE ( 'NONE', *, *, #10670, .T. ) ;
#12140 = VERTEX_POINT ( 'NONE', #11070 ) ;
#12141 = EDGE_CURVE ( 'NONE', #1896, #13924, #13578, .T. ) ;
#12142 = DIRECTION ( 'NONE',  ( 0.000000000000000000, 0.000000000000000000, -1.000000000000000000 ) ) ;
#12143 = VERTEX_POINT ( 'NONE', #4 ) ;
#12144 = DIRECTION ( 'NONE',  ( 0.000000000000000000, 0.000000000000000000, -1.000000000000000000 ) ) ;
#12145 = CARTESIAN_POINT ( 'NONE',  ( -6.473970235329672780E-16, -4.862606272033106691, -3.745885042887442395 ) ) ;
#12146 = EDGE_LOOP ( 'NONE', ( #3743, #13703, #6896 ) ) ;
#12147 = CARTESIAN_POINT ( 'NONE',  ( -31.74999999999995737, 0.000000000000000000, 0.000000000000000000 ) ) ;
#12148 = DIRECTION ( 'NONE',  ( 0.000000000000000000, 0.000000000000000000, 1.000000000000000000 ) ) ;
#12149 = DIRECTION ( 'NONE',  ( 1.000000000000000000, 0.000000000000000000, 0.000000000000000000 ) ) ;
#12150 = CARTESIAN_POINT ( 'NONE',  ( 4.999999999999999112, -8.660254037844389075, 200.0000000000000000 ) ) ;
#12151 = ADVANCED_BREP_SHAPE_REPRESENTATION ( '', ( #8769, #14039 ), #1206 ) ;
#12152 = ORIENTED_EDGE ( 'NONE', *, *, #4639, .T. ) ;
#12153 =( REPRESENTATION_RELATIONSHIP ('NONE','NONE', #11251, #11637 ) REPRESENTATION_RELATIONSHIP_WITH_TRANSFORMATION ( #6013 )SHAPE_REPRESENTATION_RELATIONSHIP( ) );
#12154 = EDGE_CURVE ( 'NONE', #4579, #12140, #4466, .T. ) ;
#12155 = DIRECTION ( 'NONE',  ( -0.000000000000000000, -0.000000000000000000, 1.000000000000000000 ) ) ;
#12156 = ADVANCED_FACE ( 'NONE', ( #13298 ), #4317, .F. ) ;
#12157 = CLOSED_SHELL ( 'NONE', ( #3393, #8972, #11276, #10168, #9122, #8439, #12320, #9258, #853, #1055, #3947, #12250, #6002, #5354, #10193, #10504, #1078, #13140, #9156, #2467, #13323, #506, #7732, #273, #2745, #8808, #4626 ) ) ;
#12158 = DIRECTION ( 'NONE',  ( 0.000000000000000000, 0.000000000000000000, -1.000000000000000000 ) ) ;
#12159 = DIRECTION ( 'NONE',  ( 0.8949343913984143528, -1.699539276894113739E-15, 0.4461977533474921764 ) ) ;
#12160 = EDGE_LOOP ( 'NONE', ( #12458, #11589 ) ) ;
#12161 = CARTESIAN_POINT ( 'NONE',  ( 386.6666666666666288, -14.99999999999999822, 222.5000000000000853 ) ) ;
#12162 = CARTESIAN_POINT ( 'NONE',  ( 3.678949249685231848, 0.000000000000000000, 0.000000000000000000 ) ) ;
#12163 = EDGE_CURVE ( 'NONE', #9002, #3958, #12636, .T. ) ;
#12164 = EDGE_CURVE ( 'NONE', #5764, #8357, #10394, .T. ) ;
#12165 = DIRECTION ( 'NONE',  ( 0.000000000000000000, -1.000000000000000000, 0.000000000000000000 ) ) ;
#12166 = DIRECTION ( 'NONE',  ( -1.000000000000000000, 0.000000000000000000, 0.000000000000000000 ) ) ;
#12167 = AXIS2_PLACEMENT_3D ( 'NONE', #6091, #6234, #8254 ) ;
#12168 = EDGE_CURVE ( 'NONE', #11990, #5253, #6645, .T. ) ;
#12169 = ITEM_DEFINED_TRANSFORMATION ( 'NONE', 'NONE', #7234,  #14039 ) ;
#12170 = EDGE_LOOP ( 'NONE', ( #1680, #2306, #279 ) ) ;
#12171 = CARTESIAN_POINT ( 'NONE',  ( 3.333333333333332593, 2.694301256218250007, -3.300726591567078483 ) ) ;
#12172 = EDGE_LOOP ( 'NONE', ( #4263, #9257, #6893, #4869, #3650, #13216 ) ) ;
#12173 = DIRECTION ( 'NONE',  ( 0.000000000000000000, 1.000000000000000000, 0.000000000000000000 ) ) ;
#12174 = CIRCLE ( 'NONE', #9862, 9.999999999999998224 ) ;
#12175 = VECTOR ( 'NONE', #9046, 1000.000000000000000 ) ;
#12176 = ORIENTED_EDGE ( 'NONE', *, *, #10670, .F. ) ;
#12177 = ORIENTED_EDGE ( 'NONE', *, *, #344, .T. ) ;
#12178 = CARTESIAN_POINT ( 'NONE',  ( 297.3499999999999659, -75.00000000000008527, -190.0000000000000000 ) ) ;
#12179 = CARTESIAN_POINT ( 'NONE',  ( 2.500000000000000000, 1.178949249685213863, -2.042000000000001148 ) ) ;
#12180 = CARTESIAN_POINT ( 'NONE',  ( 2.500000000000000000, 1.178949249685212974, -2.042000000000001148 ) ) ;
#12181 = DIRECTION ( 'NONE',  ( 0.000000000000000000, 0.000000000000000000, 1.000000000000000000 ) ) ;
#12182 = CARTESIAN_POINT ( 'NONE',  ( 119.9999999999999147, -225.0010000000000048, 169.9999999999999716 ) ) ;
#12183 = DIRECTION ( 'NONE',  ( -0.000000000000000000, 0.000000000000000000, 1.000000000000000000 ) ) ;
#12184 = PRESENTATION_STYLE_ASSIGNMENT (( #13408 ) ) ;
#12185 = CARTESIAN_POINT ( 'NONE',  ( 242.5000000000000000, -90.00000000000007105, 55.00000000000001421 ) ) ;
#12186 = DIRECTION ( 'NONE',  ( 0.000000000000000000, 0.000000000000000000, -1.000000000000000000 ) ) ;
#12187 = CIRCLE ( 'NONE', #11724, 1.050000000000000488 ) ;
#12188 = VERTEX_POINT ( 'NONE', #11345 ) ;
#12189 = ORIENTED_EDGE ( 'NONE', *, *, #11986, .T. ) ;
#12190 = CIRCLE ( 'NONE', #12882, 2.649999999999985700 ) ;
#12191 = DIRECTION ( 'NONE',  ( 0.000000000000000000, 1.224646799147353207E-16, -1.000000000000000000 ) ) ;
#12192 = ORIENTED_EDGE ( 'NONE', *, *, #13832, .T. ) ;
#12193 = DIRECTION ( 'NONE',  ( -0.000000000000000000, 0.000000000000000000, 1.000000000000000000 ) ) ;
#12194 = VECTOR ( 'NONE', #3897, 1000.000000000000000 ) ;
#12195 = EDGE_CURVE ( 'NONE', #12966, #2887, #9892, .T. ) ;
#12196 = EDGE_LOOP ( 'NONE', ( #5634, #13865, #10860, #1742 ) ) ;
#12197 = CARTESIAN_POINT ( 'NONE',  ( 269.0000000000000000, 8.660254037844390851, 199.9990000000000236 ) ) ;
#12198 = ORIENTED_EDGE ( 'NONE', *, *, #2380, .F. ) ;
#12200 = FACE_OUTER_BOUND ( 'NONE', #1462, .T. ) ;
#12199 = VECTOR ( 'NONE', #7455, 1000.000000000000000 ) ;
#12201 = VECTOR ( 'NONE', #13873, 1000.000000000000000 ) ;
#12202 = CARTESIAN_POINT ( 'NONE',  ( 4.000000000000000000, -2.309401076758514915, -3.433295621305383349 ) ) ;
#12203 = CARTESIAN_POINT ( 'NONE',  ( 219.9999999999999716, -20.00000000000000000, -222.5000000000000853 ) ) ;
#12204 = DIRECTION ( 'NONE',  ( -1.000000000000000000, -0.000000000000000000, -0.000000000000000000 ) ) ;
#12205 = FACE_OUTER_BOUND ( 'NONE', #11063, .T. ) ;
#12206 = DIRECTION ( 'NONE',  ( 0.000000000000000000, 0.000000000000000000, -1.000000000000000000 ) ) ;
#12207 = AXIS2_PLACEMENT_3D ( 'NONE', #6842, #7987, #2356 ) ;
#12208 = VERTEX_POINT ( 'NONE', #4892 ) ;
#12209 = ORIENTED_EDGE ( 'NONE', *, *, #2279, .F. ) ;
#12210 = CIRCLE ( 'NONE', #12901, 4.000000000000000000 ) ;
#12212 = FACE_OUTER_BOUND ( 'NONE', #6384, .T. ) ;
#12211 = VECTOR ( 'NONE', #1009, 1000.000000000000000 ) ;
#12213 = CIRCLE ( 'NONE', #11297, 1.037871761867652065 ) ;
#12214 = ADVANCED_FACE ( 'NONE', ( #13794 ), #12498, .T. ) ;
#12215 = EDGE_LOOP ( 'NONE', ( #13674, #11166 ) ) ;
#12216 = CARTESIAN_POINT ( 'NONE',  ( -13.50000000000000000, 1.653273178848926867E-15, 186.0000000000000000 ) ) ;
#12217 = DIRECTION ( 'NONE',  ( 0.000000000000000000, 0.8660254037844380415, -0.5000000000000012212 ) ) ;
#12218 = SURFACE_STYLE_FILL_AREA ( #4400 ) ;
#12219 = AXIS2_PLACEMENT_3D ( 'NONE', #10849, #7637, #1095 ) ;
#12220 = ORIENTED_EDGE ( 'NONE', *, *, #10124, .F. ) ;
#12221 = CIRCLE ( 'NONE', #6196, 7.864440107515624945 ) ;
#12222 = FACE_BOUND ( 'NONE', #12595, .T. ) ;
#12223 = CARTESIAN_POINT ( 'NONE',  ( -30.00000000000002842, -25.00000000000000000, 250.0000000000000000 ) ) ;
#12224 = EDGE_CURVE ( 'NONE', #11346, #2397, #4328, .T. ) ;
#12225 = AXIS2_PLACEMENT_3D ( 'NONE', #7176, #14066, #7472 ) ;
#12226 = DIRECTION ( 'NONE',  ( 1.000000000000000000, 0.000000000000000000, 0.000000000000000000 ) ) ;
#12227 = AXIS2_PLACEMENT_3D ( 'NONE', #13059, #7402, #3134 ) ;
#12228 = DIRECTION ( 'NONE',  ( 0.000000000000000000, 0.000000000000000000, -1.000000000000000000 ) ) ;
#12229 = ORIENTED_EDGE ( 'NONE', *, *, #9227, .T. ) ;
#12230 = AXIS2_PLACEMENT_3D ( 'NONE', #5701, #3536, #2438 ) ;
#12231 = DIRECTION ( 'NONE',  ( 1.000000000000000000, 0.000000000000000000, 0.000000000000000000 ) ) ;
#12232 = VECTOR ( 'NONE', #12948, 1000.000000000000000 ) ;
#12233 = CARTESIAN_POINT ( 'NONE',  ( -294.9999999999999432, -95.00000000000008527, 39.99999999999997868 ) ) ;
#12234 = ORIENTED_EDGE ( 'NONE', *, *, #9777, .F. ) ;
#12235 = CARTESIAN_POINT ( 'NONE',  ( 1.312671235360372224, 3.860931062424219462, -0.05923475698270440348 ) ) ;
#12236 = CARTESIAN_POINT ( 'NONE',  ( 5.000000000000000888, 0.000000000000000000, 0.000000000000000000 ) ) ;
#12237 = EDGE_CURVE ( 'NONE', #2628, #5131, #13575, .T. ) ;
#12238 = PRODUCT_DEFINITION ( 'UNKNOWN', '', #10494, #7114 ) ;
#12239 = CARTESIAN_POINT ( 'NONE',  ( 140.0000000000000000, -75.00000000000008527, 190.0000000000000000 ) ) ;
#12240 = CARTESIAN_POINT ( 'NONE',  ( 136.6666666666666288, -10.00000000000000000, 222.5000000000000853 ) ) ;
#12241 = EDGE_CURVE ( 'NONE', #6402, #9645, #2568, .T. ) ;
#12242 =( REPRESENTATION_RELATIONSHIP ('NONE','NONE', #11251, #11637 ) REPRESENTATION_RELATIONSHIP_WITH_TRANSFORMATION ( #3283 )SHAPE_REPRESENTATION_RELATIONSHIP( ) );
#12243 = ITEM_DEFINED_TRANSFORMATION ( 'NONE', 'NONE', #245,  #14039 ) ;
#12244 = VECTOR ( 'NONE', #661, 1000.000000000000000 ) ;
#12245 = ORIENTED_EDGE ( 'NONE', *, *, #13580, .T. ) ;
#12246 = PLANE ( 'NONE',  #5245 ) ;
#12247 = PRODUCT_DEFINITION_SHAPE ( 'NONE', 'NONE',  #1599 ) ;
#12248 = VERTEX_POINT ( 'NONE', #3867 ) ;
#12249 = CARTESIAN_POINT ( 'NONE',  ( -4.000000000000000000, -2.309401076758515803, -0.4999999999999995559 ) ) ;
#12250 = ADVANCED_FACE ( 'NONE', ( #2639 ), #216, .T. ) ;
#12251 = ORIENTED_EDGE ( 'NONE', *, *, #12038, .F. ) ;
#12252 = VERTEX_POINT ( 'NONE', #6985 ) ;
#12253 = CARTESIAN_POINT ( 'NONE',  ( 302.5000000000000000, -36.99999999999997868, -180.0000000000000000 ) ) ;
#12254 = LINE ( 'NONE', #7535, #6634 ) ;
#12255 = DIRECTION ( 'NONE',  ( -1.000000000000000000, -0.000000000000000000, -0.000000000000000000 ) ) ;
#12256 = AXIS2_PLACEMENT_3D ( 'NONE', #11388, #9205, #2611 ) ;
#12257 = ADVANCED_FACE ( 'NONE', ( #8286 ), #4678, .T. ) ;
#12258 = DIRECTION ( 'NONE',  ( -0.000000000000000000, 1.000000000000000000, -0.000000000000000000 ) ) ;
#12259 = CARTESIAN_POINT ( 'NONE',  ( -302.4999999999999432, -75.00000000000008527, 0.000000000000000000 ) ) ;
#12260 = DIRECTION ( 'NONE',  ( 1.000000000000000000, 0.000000000000000000, 0.000000000000000000 ) ) ;
#12261 = SURFACE_SIDE_STYLE ('',( #109 ) ) ;
#12262 = DIRECTION ( 'NONE',  ( 0.000000000000000000, 0.000000000000000000, -1.000000000000000000 ) ) ;
#12263 = CONTEXT_DEPENDENT_SHAPE_REPRESENTATION ( #7964, #7638 ) ;
#12264 = CARTESIAN_POINT ( 'NONE',  ( 82.99999999999998579, 8.660254037844390851, 199.9990000000000236 ) ) ;
#12265 = ORIENTED_EDGE ( 'NONE', *, *, #2870, .T. ) ;
#12266 = VERTEX_POINT ( 'NONE', #7132 ) ;
#12267 = DIRECTION ( 'NONE',  ( 0.000000000000000000, 0.000000000000000000, 1.000000000000000000 ) ) ;
#12268 = ORIENTED_EDGE ( 'NONE', *, *, #12980, .T. ) ;
#12269 = DIRECTION ( 'NONE',  ( -1.000000000000000000, 0.000000000000000000, 0.000000000000000000 ) ) ;
#12270 = CIRCLE ( 'NONE', #8793, 0.4499999999999985678 ) ;
#12271 = EDGE_CURVE ( 'NONE', #3312, #11069, #12573, .T. ) ;
#12272 = EDGE_LOOP ( 'NONE', ( #5591, #4878, #13037, #3785 ) ) ;
#12273 = EDGE_CURVE ( 'NONE', #1770, #3461, #1320, .T. ) ;
#12274 = FACE_OUTER_BOUND ( 'NONE', #8967, .T. ) ;
#12275 = ORIENTED_EDGE ( 'NONE', *, *, #12433, .T. ) ;
#12276 = PLANE ( 'NONE',  #10556 ) ;
#12277 = DIRECTION ( 'NONE',  ( 1.000000000000000000, 0.000000000000000000, 0.000000000000000000 ) ) ;
#12278 = CARTESIAN_POINT ( 'NONE',  ( 25.00000000000000000, 0.000000000000000000, 0.000000000000000000 ) ) ;
#12279 = EDGE_CURVE ( 'NONE', #8279, #3380, #1604, .T. ) ;
#12280 = DIRECTION ( 'NONE',  ( 0.000000000000000000, 1.000000000000000000, -1.224646799147353207E-16 ) ) ;
#12281 = SHAPE_REPRESENTATION_RELATIONSHIP ( 'NONE' , 'NONE' ,  #2740, #12845 ) ;
#12282 = CARTESIAN_POINT ( 'NONE',  ( 0.000000000000000000, -2.349999999999999201, -0.5150000000000000133 ) ) ;
#12283 = DIRECTION ( 'NONE',  ( 6.123233995736766036E-17, 0.000000000000000000, -1.000000000000000000 ) ) ;
#12284 = DIRECTION ( 'NONE',  ( -0.8571673013836870192, 1.049727191973306873E-16, 0.5150380737757234151 ) ) ;
#12285 = ORIENTED_EDGE ( 'NONE', *, *, #8416, .T. ) ;
#12286 = VECTOR ( 'NONE', #11605, 1000.000000000000000 ) ;
#12287 = VERTEX_POINT ( 'NONE', #9312 ) ;
#12288 = AXIS2_PLACEMENT_3D ( 'NONE', #14142, #9518, #8644 ) ;
#12289 = CARTESIAN_POINT ( 'NONE',  ( -20.63749999999999574, 0.000000000000000000, 0.000000000000000000 ) ) ;
#12290 = ORIENTED_EDGE ( 'NONE', *, *, #1798, .T. ) ;
#12291 = CARTESIAN_POINT ( 'NONE',  ( 386.6666666666666288, -20.00000000000000000, 222.5000000000000853 ) ) ;
#12292 = PLANE ( 'NONE',  #12207 ) ;
#12293 = CARTESIAN_POINT ( 'NONE',  ( 0.000000000000000000, 0.000000000000000000, 0.000000000000000000 ) ) ;
#12294 = CIRCLE ( 'NONE', #12748, 5.500000000000005329 ) ;
#12295 = VECTOR ( 'NONE', #4745, 1000.000000000000000 ) ;
#12296 = FACE_OUTER_BOUND ( 'NONE', #4724, .T. ) ;
#12297 = CONICAL_SURFACE ( 'NONE', #9281, 3077.683537175319998, 1.256637061435923686 ) ;
#12298 = DIRECTION ( 'NONE',  ( 0.000000000000000000, 0.000000000000000000, 1.000000000000000000 ) ) ;
#12299 = DIRECTION ( 'NONE',  ( -0.000000000000000000, -0.000000000000000000, 1.000000000000000000 ) ) ;
#12300 = FACE_OUTER_BOUND ( 'NONE', #6942, .T. ) ;
#12301 = EDGE_CURVE ( 'NONE', #514, #8786, #13728, .T. ) ;
#12302 = EDGE_LOOP ( 'NONE', ( #11019, #13432, #6329, #4886 ) ) ;
#12303 = CIRCLE ( 'NONE', #5140, 2.649999999999985700 ) ;
#12304 = APPLICATION_CONTEXT ( 'automotive_design' ) ;
#12305 = AXIS2_PLACEMENT_3D ( 'NONE', #13875, #3952, #4755 ) ;
#12306 = CARTESIAN_POINT ( 'NONE',  ( 0.000000000000000000, 0.000000000000000000, -4.000000000000000000 ) ) ;
#12307 = CARTESIAN_POINT ( 'NONE',  ( 294.4999999999999432, -75.00000000000008527, 190.0000000000000000 ) ) ;
#12308 = DIRECTION ( 'NONE',  ( 0.000000000000000000, 1.000000000000000000, -1.224646799147353207E-16 ) ) ;
#12309 = EDGE_LOOP ( 'NONE', ( #12756, #10692, #4030, #4378, #102 ) ) ;
#12310 = AXIS2_PLACEMENT_3D ( 'NONE', #2426, #11213, #10 ) ;
#12311 = FACE_OUTER_BOUND ( 'NONE', #3466, .T. ) ;
#12312 = CARTESIAN_POINT ( 'NONE',  ( 470.0000000000000000, -20.00000000000000000, 240.0000000000000284 ) ) ;
#12313 = CARTESIAN_POINT ( 'NONE',  ( 0.000000000000000000, 0.000000000000000000, 0.000000000000000000 ) ) ;
#12314 = ORIENTED_EDGE ( 'NONE', *, *, #14111, .F. ) ;
#12315 = CARTESIAN_POINT ( 'NONE',  ( 2.500000000000000000, 1.178949249685213863, -2.042000000000001148 ) ) ;
#12316 = VECTOR ( 'NONE', #733, 1000.000000000000000 ) ;
#12317 = ORIENTED_EDGE ( 'NONE', *, *, #11275, .T. ) ;
#12318 = CIRCLE ( 'NONE', #909, 2.649999999999985700 ) ;
#12319 = CARTESIAN_POINT ( 'NONE',  ( 0.5276280594147412240, -4.314175951381924889, -3.320322319201654881 ) ) ;
#12320 = ADVANCED_FACE ( 'NONE', ( #5754, #9095 ), #6045, .T. ) ;
#12321 = EDGE_CURVE ( 'NONE', #2019, #10963, #13508, .T. ) ;
#12322 = ORIENTED_EDGE ( 'NONE', *, *, #10137, .T. ) ;
#12323 = ORIENTED_EDGE ( 'NONE', *, *, #8686, .F. ) ;
#12324 = DIRECTION ( 'NONE',  ( 0.000000000000000000, 0.000000000000000000, -1.000000000000000000 ) ) ;
#12325 = DIRECTION ( 'NONE',  ( 1.000000000000000000, 0.000000000000000000, 0.000000000000000000 ) ) ;
#12326 = DIRECTION ( 'NONE',  ( -0.8949343913984706411, 0.4461977533473793223, 0.000000000000000000 ) ) ;
#12327 = FACE_OUTER_BOUND ( 'NONE', #9759, .T. ) ;
#12328 = LINE ( 'NONE', #2393, #2459 ) ;
#12329 = AXIS2_PLACEMENT_3D ( 'NONE', #4545, #13597, #6929 ) ;
#12330 = DIRECTION ( 'NONE',  ( 1.000000000000000000, 0.000000000000000000, 0.000000000000000000 ) ) ;
#12331 = AXIS2_PLACEMENT_3D ( 'NONE', #2520, #3748, #8163 ) ;
#12332 = ORIENTED_EDGE ( 'NONE', *, *, #2655, .T. ) ;
#12333 = COLOUR_RGB ( '',0.8941176470588234615, 0.8941176470588234615, 0.8941176470588234615 ) ;
#12334 = ORIENTED_EDGE ( 'NONE', *, *, #12675, .F. ) ;
#12335 = CARTESIAN_POINT ( 'NONE',  ( 0.000000000000000000, 1.178949249685213863, -2.042000000000001148 ) ) ;
#12336 = EDGE_LOOP ( 'NONE', ( #12761, #7765 ) ) ;
#12337 = DIRECTION ( 'NONE',  ( 0.000000000000000000, 1.000000000000000000, 0.000000000000000000 ) ) ;
#12338 = EDGE_CURVE ( 'NONE', #2338, #13280, #3189, .T. ) ;
#12339 = EDGE_CURVE ( 'NONE', #3954, #8184, #11700, .T. ) ;
#12340 = AXIS2_PLACEMENT_3D ( 'NONE', #2141, #6570, #5472 ) ;
#12341 = ORIENTED_EDGE ( 'NONE', *, *, #2918, .T. ) ;
#12342 = DIRECTION ( 'NONE',  ( 0.000000000000000000, 0.000000000000000000, -1.000000000000000000 ) ) ;
#12343 = VERTEX_POINT ( 'NONE', #4082 ) ;
#12344 = CARTESIAN_POINT ( 'NONE',  ( 0.000000000000000000, 0.000000000000000000, -5.000000000000000000 ) ) ;
#12345 = VERTEX_POINT ( 'NONE', #6005 ) ;
#12346 = LINE ( 'NONE', #7702, #13148 ) ;
#12347 = MECHANICAL_DESIGN_GEOMETRIC_PRESENTATION_REPRESENTATION (  '', ( #7480 ), #3097 ) ;
#12348 = LINE ( 'NONE', #2409, #8965 ) ;
#12349 = PLANE ( 'NONE',  #4404 ) ;
#12350 = LINE ( 'NONE', #1308, #10701 ) ;
#12351 = CARTESIAN_POINT ( 'NONE',  ( 134.9999999999999432, -36.99999999999997868, -154.9999999999999716 ) ) ;
#12352 = EDGE_CURVE ( 'NONE', #8359, #14256, #14058, .T. ) ;
#12353 = EDGE_CURVE ( 'NONE', #6756, #8236, #8020, .T. ) ;
#12354 = FACE_BOUND ( 'NONE', #6631, .T. ) ;
#12355 = VECTOR ( 'NONE', #1317, 1000.000000000000000 ) ;
#12356 = ORIENTED_EDGE ( 'NONE', *, *, #11116, .T. ) ;
#12357 = EDGE_CURVE ( 'NONE', #11600, #11926, #1829, .T. ) ;
#12358 = EDGE_CURVE ( 'NONE', #11122, #2563, #363, .T. ) ;
#12359 = ORIENTED_EDGE ( 'NONE', *, *, #1917, .T. ) ;
#12360 = EDGE_LOOP ( 'NONE', ( #10213, #13495, #8078, #9146 ) ) ;
#12361 = LINE ( 'NONE', #7103, #3779 ) ;
#12362 = ORIENTED_EDGE ( 'NONE', *, *, #8992, .T. ) ;
#12363 = CARTESIAN_POINT ( 'NONE',  ( 470.0000000000000000, 0.000000000000000000, 200.0000000000000000 ) ) ;
#12364 = CARTESIAN_POINT ( 'NONE',  ( 2.740000000000000213, 0.9838866223910003317, 0.5149999999999999023 ) ) ;
#12365 = CARTESIAN_POINT ( 'NONE',  ( 7.345657149124971141, -1.312408941149200814, 2.762944903268657774E-16 ) ) ;
#12366 = DIRECTION ( 'NONE',  ( -1.000000000000000000, 0.000000000000000000, 0.000000000000000000 ) ) ;
#12367 = CARTESIAN_POINT ( 'NONE',  ( 24.55500000000002103, 3.061616997868384620E-16, -2.500000000000001332 ) ) ;
#12368 = CARTESIAN_POINT ( 'NONE',  ( 4.999999999999999112, -8.660254037844389075, 210.0000000000000000 ) ) ;
#12369 = PRODUCT_DEFINITION_SHAPE ( 'NONE', 'NONE',  #14316 ) ;
#12370 = LINE ( 'NONE', #12511, #7979 ) ;
#12371 = ORIENTED_EDGE ( 'NONE', *, *, #9883, .F. ) ;
#12372 =( NAMED_UNIT ( * ) SI_UNIT ( $, .STERADIAN. ) SOLID_ANGLE_UNIT ( ) );
#12373 = DIRECTION ( 'NONE',  ( -0.000000000000000000, -0.000000000000000000, 1.000000000000000000 ) ) ;
#12374 = DIRECTION ( 'NONE',  ( 0.8571673013836870192, 0.000000000000000000, 0.5150380737757234151 ) ) ;
#12375 = CARTESIAN_POINT ( 'NONE',  ( 0.000000000000000000, -15.00000000000000000, 0.000000000000000000 ) ) ;
#12376 = EDGE_CURVE ( 'NONE', #11681, #2861, #10593, .T. ) ;
#12377 = ORIENTED_EDGE ( 'NONE', *, *, #6565, .F. ) ;
#12378 = CARTESIAN_POINT ( 'NONE',  ( 2.740000000000000213, 0.6774776749089228556, 0.5149999999999997913 ) ) ;
#12379 = DIRECTION ( 'NONE',  ( 0.000000000000000000, 1.000000000000000000, -1.471414886128461471E-15 ) ) ;
#12380 = DIRECTION ( 'NONE',  ( 1.000000000000000000, 0.000000000000000000, 0.000000000000000000 ) ) ;
#12381 = CIRCLE ( 'NONE', #7517, 4.750000000000000000 ) ;
#12382 = ORIENTED_EDGE ( 'NONE', *, *, #4615, .F. ) ;
#12383 = CARTESIAN_POINT ( 'NONE',  ( -20.63749999999999574, 0.000000000000000000, -13.50000000000000355 ) ) ;
#12384 = ORIENTED_EDGE ( 'NONE', *, *, #517, .F. ) ;
#12385 = CARTESIAN_POINT ( 'NONE',  ( 259.0000000000000000, 8.660254037844390851, 200.0000000000000000 ) ) ;
#12386 = VERTEX_POINT ( 'NONE', #7271 ) ;
#12387 = ORIENTED_EDGE ( 'NONE', *, *, #2224, .F. ) ;
#12388 = DIRECTION ( 'NONE',  ( -1.000000000000000000, -0.000000000000000000, -0.000000000000000000 ) ) ;
#12389 = DIRECTION ( 'NONE',  ( 0.000000000000000000, 0.4999999999999993894, -0.8660254037844389297 ) ) ;
#12390 = AXIS2_PLACEMENT_3D ( 'NONE', #5689, #1256, #9105 ) ;
#12391 = DIRECTION ( 'NONE',  ( 1.000000000000000000, 0.000000000000000000, 0.000000000000000000 ) ) ;
#12392 = CARTESIAN_POINT ( 'NONE',  ( 2.740000000000000213, 0.000000000000000000, 0.000000000000000000 ) ) ;
#12393 = CYLINDRICAL_SURFACE ( 'NONE', #3308, 10.72500000000000142 ) ;
#12394 = DIRECTION ( 'NONE',  ( 1.000000000000000000, 0.000000000000000000, 0.000000000000000000 ) ) ;
#12395 = FILL_AREA_STYLE ('',( #9423 ) ) ;
#12396 = CARTESIAN_POINT ( 'NONE',  ( -1.800000000000002931, 0.000000000000000000, -13.50000000000000355 ) ) ;
#12397 = EDGE_CURVE ( 'NONE', #3017, #8136, #5191, .T. ) ;
#12398 = CONTEXT_DEPENDENT_SHAPE_REPRESENTATION ( #14183, #1585 ) ;
#12399 = ORIENTED_EDGE ( 'NONE', *, *, #3152, .T. ) ;
#12400 = VERTEX_POINT ( 'NONE', #5324 ) ;
#12401 = DIRECTION ( 'NONE',  ( -0.000000000000000000, -0.000000000000000000, -1.000000000000000000 ) ) ;
#12402 = ORIENTED_EDGE ( 'NONE', *, *, #9850, .F. ) ;
#12403 = VECTOR ( 'NONE', #7809, 1000.000000000000000 ) ;
#12404 = CARTESIAN_POINT ( 'NONE',  ( 144.9999999999999716, -64.99999999999997158, 10.00000000000000000 ) ) ;
#12405 = ADVANCED_FACE ( 'NONE', ( #653 ), #6115, .F. ) ;
#12406 = ORIENTED_EDGE ( 'NONE', *, *, #5126, .F. ) ;
#12407 = DIRECTION ( 'NONE',  ( -0.000000000000000000, -1.000000000000000000, -0.000000000000000000 ) ) ;
#12408 = ORIENTED_EDGE ( 'NONE', *, *, #3659, .F. ) ;
#12409 = LINE ( 'NONE', #5812, #2216 ) ;
#12410 = CARTESIAN_POINT ( 'NONE',  ( 140.0000000000000000, -75.00000000000008527, -190.0000000000000000 ) ) ;
#12411 = CARTESIAN_POINT ( 'NONE',  ( 0.000000000000000000, 0.000000000000000000, -190.0000000000000000 ) ) ;
#12412 = CARTESIAN_POINT ( 'NONE',  ( -4.000000000000000000, 2.309401076758498483, -3.433295621305379353 ) ) ;
#12413 = CARTESIAN_POINT ( 'NONE',  ( -20.63749999999999929, 0.000000000000000000, 0.000000000000000000 ) ) ;
#12414 = EDGE_CURVE ( 'NONE', #11189, #6109, #9675, .T. ) ;
#12415 = DIRECTION ( 'NONE',  ( 6.123233995736766036E-17, 0.000000000000000000, -1.000000000000000000 ) ) ;
#12416 = PRODUCT_RELATED_PRODUCT_CATEGORY ( 'part', '', ( #1347 ) ) ;
#12417 = FACE_BOUND ( 'NONE', #9880, .T. ) ;
#12418 = ORIENTED_EDGE ( 'NONE', *, *, #13053, .T. ) ;
#12419 = ORIENTED_EDGE ( 'NONE', *, *, #2380, .T. ) ;
#12420 = AXIS2_PLACEMENT_3D ( 'NONE', #2109, #4224, #14077 ) ;
#12421 = ORIENTED_EDGE ( 'NONE', *, *, #10092, .T. ) ;
#12422 = FACE_OUTER_BOUND ( 'NONE', #9213, .T. ) ;
#12423 = AXIS2_PLACEMENT_3D ( 'NONE', #12161, #13654, #8141 ) ;
#12424 = EDGE_LOOP ( 'NONE', ( #2725, #8312 ) ) ;
#12425 = CARTESIAN_POINT ( 'NONE',  ( 82.99999999999998579, -8.660254037844389075, 200.0000000000000000 ) ) ;
#12426 = ORIENTED_EDGE ( 'NONE', *, *, #9838, .T. ) ;
#12427 = CARTESIAN_POINT ( 'NONE',  ( 0.000000000000000000, 0.000000000000000000, 0.000000000000000000 ) ) ;
#12428 = EDGE_CURVE ( 'NONE', #7102, #5706, #14008, .T. ) ;
#12429 = ADVANCED_FACE ( 'NONE', ( #3006, #6340 ), #9748, .F. ) ;
#12430 = AXIS2_PLACEMENT_3D ( 'NONE', #3021, #6205, #13883 ) ;
#12431 = SURFACE_STYLE_USAGE ( .BOTH. , #9317 ) ;
#12432 =( REPRESENTATION_RELATIONSHIP ('NONE','NONE', #11251, #13104 ) REPRESENTATION_RELATIONSHIP_WITH_TRANSFORMATION ( #12755 )SHAPE_REPRESENTATION_RELATIONSHIP( ) );
#12433 = EDGE_CURVE ( 'NONE', #7650, #9829, #4236, .T. ) ;
#12434 = DIRECTION ( 'NONE',  ( 0.000000000000000000, 0.000000000000000000, 1.000000000000000000 ) ) ;
#12435 = DIRECTION ( 'NONE',  ( -1.000000000000000000, 0.000000000000000000, 0.000000000000000000 ) ) ;
#12436 = AXIS2_PLACEMENT_3D ( 'NONE', #9337, #11434, #5847 ) ;
#12437 = DIRECTION ( 'NONE',  ( 0.000000000000000000, 0.000000000000000000, -1.000000000000000000 ) ) ;
#12438 = CARTESIAN_POINT ( 'NONE',  ( -20.63749999999999574, 0.000000000000000000, 0.000000000000000000 ) ) ;
#12439 = AXIS2_PLACEMENT_3D ( 'NONE', #13942, #10694, #7422 ) ;
#12440 = ORIENTED_EDGE ( 'NONE', *, *, #9608, .F. ) ;
#12441 = CIRCLE ( 'NONE', #8021, 12.77499999999999858 ) ;
#12442 = PRESENTATION_STYLE_ASSIGNMENT (( #11358 ) ) ;
#12443 = AXIS2_PLACEMENT_3D ( 'NONE', #942, #5404, #12206 ) ;
#12444 = CARTESIAN_POINT ( 'NONE',  ( -140.0000000000000000, -95.00000000000008527, -14.14213562373090127 ) ) ;
#12445 = DIRECTION ( 'NONE',  ( 1.000000000000000000, 0.000000000000000000, 0.000000000000000000 ) ) ;
#12446 = AXIS2_PLACEMENT_3D ( 'NONE', #6697, #10095, #7906 ) ;
#12447 = EDGE_CURVE ( 'NONE', #10068, #1338, #8426, .T. ) ;
#12448 = DIRECTION ( 'NONE',  ( -0.000000000000000000, -0.000000000000000000, 1.000000000000000000 ) ) ;
#12449 = EDGE_LOOP ( 'NONE', ( #5528, #606, #10998, #777 ) ) ;
#12450 = AXIS2_PLACEMENT_3D ( 'NONE', #8188, #12407, #1297 ) ;
#12451 = AXIS2_PLACEMENT_3D ( 'NONE', #991, #5651, #5582 ) ;
#12452 = DIRECTION ( 'NONE',  ( -1.000000000000000000, 0.000000000000000000, 0.000000000000000000 ) ) ;
#12453 = ADVANCED_FACE ( 'NONE', ( #2927 ), #7341, .F. ) ;
#12454 = CARTESIAN_POINT ( 'NONE',  ( 303.3333333333333144, -20.00000000000000000, -222.5000000000000853 ) ) ;
#12455 = DIRECTION ( 'NONE',  ( 0.000000000000000000, 0.000000000000000000, 1.000000000000000000 ) ) ;
#12456 = AXIS2_PLACEMENT_3D ( 'NONE', #10461, #8277, #4885 ) ;
#12457 = AXIS2_PLACEMENT_3D ( 'NONE', #11909, #8484, #3137 ) ;
#12458 = ORIENTED_EDGE ( 'NONE', *, *, #12168, .T. ) ;
#12459 = AXIS2_PLACEMENT_3D ( 'NONE', #10785, #10714, #13965 ) ;
#12460 = CARTESIAN_POINT ( 'NONE',  ( 2.500000000000000000, -1.178949249685213863, 2.042000000000002924 ) ) ;
#12461 = EDGE_LOOP ( 'NONE', ( #5071, #5425, #7605, #751 ) ) ;
#12462 = LINE ( 'NONE', #10006, #2331 ) ;
#12463 = ORIENTED_EDGE ( 'NONE', *, *, #1948, .T. ) ;
#12464 = ORIENTED_EDGE ( 'NONE', *, *, #14091, .F. ) ;
#12465 = DIRECTION ( 'NONE',  ( 0.000000000000000000, 0.4999999999999993339, -0.8660254037844390407 ) ) ;
#12466 = CARTESIAN_POINT ( 'NONE',  ( -2.742827927723112236, -3.035229711105190464, -3.433252694550595230 ) ) ;
#12467 = FILL_AREA_STYLE ('',( #8028 ) ) ;
#12468 = VECTOR ( 'NONE', #9461, 1000.000000000000000 ) ;
#12469 = CARTESIAN_POINT ( 'NONE',  ( 302.6499999999999204, -95.00000000000008527, 190.0000000000000000 ) ) ;
#12470 = DIRECTION ( 'NONE',  ( -1.000000000000000000, 0.000000000000000000, 0.000000000000000000 ) ) ;
#12471 = LINE ( 'NONE', #3767, #8013 ) ;
#12472 = CARTESIAN_POINT ( 'NONE',  ( 3.349226789952652439, 2.685125164760731487, -0.2236248678334773199 ) ) ;
#12473 = ORIENTED_EDGE ( 'NONE', *, *, #8204, .F. ) ;
#12474 = EDGE_CURVE ( 'NONE', #5437, #9413, #8253, .T. ) ;
#12475 = ORIENTED_EDGE ( 'NONE', *, *, #4388, .T. ) ;
#12476 = DIRECTION ( 'NONE',  ( -0.000000000000000000, 1.000000000000000000, -0.000000000000000000 ) ) ;
#12477 = ORIENTED_EDGE ( 'NONE', *, *, #8346, .F. ) ;
#12478 = CARTESIAN_POINT ( 'NONE',  ( 134.5000000000000000, -95.00000000000008527, -190.0000000000000000 ) ) ;
#12479 = ORIENTED_EDGE ( 'NONE', *, *, #9528, .T. ) ;
#12480 = PLANE ( 'NONE',  #11516 ) ;
#12481 = ORIENTED_EDGE ( 'NONE', *, *, #7232, .T. ) ;
#12482 = CIRCLE ( 'NONE', #651, 2.500000000000000888 ) ;
#12483 = CARTESIAN_POINT ( 'NONE',  ( -299.9999999999999432, -95.00000000000008527, 354.1421356237308942 ) ) ;
#12484 = PRODUCT_DEFINITION_SHAPE ( 'NONE', 'NONE',  #1870 ) ;
#12485 = DIRECTION ( 'NONE',  ( 0.000000000000000000, 0.000000000000000000, 1.000000000000000000 ) ) ;
#12486 = ORIENTED_EDGE ( 'NONE', *, *, #10756, .T. ) ;
#12487 = DIRECTION ( 'NONE',  ( -2.775557561562892929E-15, 1.000000000000000000, 0.000000000000000000 ) ) ;
#12488 = SURFACE_STYLE_FILL_AREA ( #5023 ) ;
#12489 = LINE ( 'NONE', #8057, #10356 ) ;
#12490 =( REPRESENTATION_RELATIONSHIP ('NONE','NONE', #11251, #3832 ) REPRESENTATION_RELATIONSHIP_WITH_TRANSFORMATION ( #13641 )SHAPE_REPRESENTATION_RELATIONSHIP( ) );
#12491 = VERTEX_POINT ( 'NONE', #11630 ) ;
#12492 = VECTOR ( 'NONE', #12165, 1000.000000000000000 ) ;
#12493 = ORIENTED_EDGE ( 'NONE', *, *, #6579, .F. ) ;
#12494 = ORIENTED_EDGE ( 'NONE', *, *, #614, .T. ) ;
#12495 = DIRECTION ( 'NONE',  ( -0.000000000000000000, -1.000000000000000000, -0.000000000000000000 ) ) ;
#12496 = AXIS2_PLACEMENT_3D ( 'NONE', #9371, #6903, #7908 ) ;
#12497 = ORIENTED_EDGE ( 'NONE', *, *, #11029, .F. ) ;
#12498 = SPHERICAL_SURFACE ( 'NONE', #10812, 8.000000000000000000 ) ;
#12499 = ORIENTED_EDGE ( 'NONE', *, *, #9393, .F. ) ;
#12500 = ADVANCED_FACE ( 'NONE', ( #9458 ), #5282, .F. ) ;
#12501 = CARTESIAN_POINT ( 'NONE',  ( 0.2500000000000002220, 0.000000000000000000, 4.250000000000000000 ) ) ;
#12502 = EDGE_CURVE ( 'NONE', #8482, #4614, #2860, .T. ) ;
#12503 = CARTESIAN_POINT ( 'NONE',  ( -302.4999999999999432, -75.00000000000008527, 339.9999999999999432 ) ) ;
#12504 = DIRECTION ( 'NONE',  ( -0.000000000000000000, -0.000000000000000000, -1.000000000000000000 ) ) ;
#12505 = VECTOR ( 'NONE', #6358, 1000.000000000000114 ) ;
#12506 = FACE_OUTER_BOUND ( 'NONE', #3917, .T. ) ;
#12507 = CIRCLE ( 'NONE', #2316, 5.500000000000005329 ) ;
#12508 = DIRECTION ( 'NONE',  ( 0.000000000000000000, 0.000000000000000000, 1.000000000000000000 ) ) ;
#12509 = CARTESIAN_POINT ( 'NONE',  ( 119.9999999999999147, -24.99999999999999289, -169.9999999999999716 ) ) ;
#12510 = VECTOR ( 'NONE', #8126, 1000.000000000000000 ) ;
#12511 = CARTESIAN_POINT ( 'NONE',  ( 347.0000000000000000, 8.660254037844390851, 205.0000000000000284 ) ) ;
#12512 = EDGE_CURVE ( 'NONE', #10809, #5615, #2264, .T. ) ;
#12513 = EDGE_LOOP ( 'NONE', ( #14004, #170, #8662, #12234, #11430 ) ) ;
#12514 = DIRECTION ( 'NONE',  ( 1.000000000000000000, 0.000000000000000000, 0.000000000000000000 ) ) ;
#12515 = EDGE_CURVE ( 'NONE', #9071, #5006, #11982, .T. ) ;
#12516 = DIRECTION ( 'NONE',  ( 1.000000000000000000, 0.000000000000000000, 0.000000000000000000 ) ) ;
#12517 = EDGE_CURVE ( 'NONE', #8094, #8759, #2120, .T. ) ;
#12518 = LINE ( 'NONE', #1476, #2742 ) ;
#12519 = VERTEX_POINT ( 'NONE', #5665 ) ;
#12520 = AXIS2_PLACEMENT_3D ( 'NONE', #4999, #5080, #7308 ) ;
#12521 = EDGE_CURVE ( 'NONE', #11569, #8359, #122, .T. ) ;
#12522 = CARTESIAN_POINT ( 'NONE',  ( 297.3499999999999659, -75.00000000000008527, 186.2999999999999829 ) ) ;
#12523 = CYLINDRICAL_SURFACE ( 'NONE', #9482, 2.649999999999985700 ) ;
#12524 = DIRECTION ( 'NONE',  ( 0.000000000000000000, 0.000000000000000000, 1.000000000000000000 ) ) ;
#12525 = AXIS2_PLACEMENT_3D ( 'NONE', #7003, #11431, #1404 ) ;
#12526 = CARTESIAN_POINT ( 'NONE',  ( 219.9999999999999147, -85.00000000000009948, -18.00000000000000355 ) ) ;
#12527 = EDGE_CURVE ( 'NONE', #9004, #1008, #3294, .T. ) ;
#12528 = ADVANCED_FACE ( 'NONE', ( #4586 ), #13144, .F. ) ;
#12529 = ADVANCED_FACE ( 'NONE', ( #13348, #12274 ), #5394, .T. ) ;
#12530=STYLED_ITEM('',(#14389),#3574);
#12531 = ORIENTED_EDGE ( 'NONE', *, *, #11728, .T. ) ;
#12532 = CARTESIAN_POINT ( 'NONE',  ( -1.312671235360383548, -3.860931062424228788, -0.05923475698271369466 ) ) ;
#12533 = DIRECTION ( 'NONE',  ( 1.000000000000000000, 0.000000000000000000, 0.000000000000000000 ) ) ;
#12534 = EDGE_CURVE ( 'NONE', #4256, #14079, #3639, .T. ) ;
#12535 = VECTOR ( 'NONE', #11277, 1000.000000000000000 ) ;
#12536 = ORIENTED_EDGE ( 'NONE', *, *, #13435, .T. ) ;
#12537 = EDGE_LOOP ( 'NONE', ( #5125, #13606 ) ) ;
#12538 = CARTESIAN_POINT ( 'NONE',  ( 197.5000000000000000, -90.00000000000007105, 50.00000000000001421 ) ) ;
#12539 = CARTESIAN_POINT ( 'NONE',  ( -1.274258131565027874, -3.883108878240886241, -3.220599429844051009 ) ) ;
#12540 = DIRECTION ( 'NONE',  ( 1.000000000000000000, 0.000000000000000000, 0.000000000000000000 ) ) ;
#12541=STYLED_ITEM('',(#14396),#3714);
#12542 = CARTESIAN_POINT ( 'NONE',  ( 142.6500000000000057, -75.00000000000008527, -169.9999999999999716 ) ) ;
#12543 = LINE ( 'NONE', #5934, #3319 ) ;
#12544 = FACE_OUTER_BOUND ( 'NONE', #9886, .T. ) ;
#12545 = CARTESIAN_POINT ( 'NONE',  ( 0.000000000000000000, 0.000000000000000000, 190.0000000000000000 ) ) ;
#12546 = VECTOR ( 'NONE', #7752, 1000.000000000000000 ) ;
#12547 = ORIENTED_EDGE ( 'NONE', *, *, #12273, .F. ) ;
#12548 = ORIENTED_EDGE ( 'NONE', *, *, #62, .F. ) ;
#12549 = PLANE ( 'NONE',  #6611 ) ;
#12550 = PRESENTATION_LAYER_ASSIGNMENT (  '', '', ( #6765 ) ) ;
#12551 = ORIENTED_EDGE ( 'NONE', *, *, #11090, .T. ) ;
#12552 = DIRECTION ( 'NONE',  ( 0.000000000000000000, -1.000000000000000000, 1.287488025362403787E-15 ) ) ;
#12553 = ORIENTED_EDGE ( 'NONE', *, *, #2670, .F. ) ;
#12554 = CARTESIAN_POINT ( 'NONE',  ( 307.5000000000000000, -36.99999999999997868, -180.0000000000000000 ) ) ;
#12555 = ORIENTED_EDGE ( 'NONE', *, *, #4954, .T. ) ;
#12556 = LINE ( 'NONE', #8633, #8726 ) ;
#12557 = DIRECTION ( 'NONE',  ( -1.000000000000000000, 0.000000000000000000, 0.000000000000000000 ) ) ;
#12559 = ORIENTED_EDGE ( 'NONE', *, *, #530, .T. ) ;
#12558 = AXIS2_PLACEMENT_3D ( 'NONE', #4911, #5059, #10413 ) ;
#12560 = FACE_OUTER_BOUND ( 'NONE', #9088, .T. ) ;
#12561 = EDGE_CURVE ( 'NONE', #12491, #678, #5457, .T. ) ;
#12562 = DIRECTION ( 'NONE',  ( -0.000000000000000000, -0.000000000000000000, 1.000000000000000000 ) ) ;
#12563 = AXIS2_PLACEMENT_3D ( 'NONE', #7077, #1555, #13459 ) ;
#12564 =( LENGTH_UNIT ( ) NAMED_UNIT ( * ) SI_UNIT ( .MILLI., .METRE. ) );
#12565 = FACE_BOUND ( 'NONE', #10792, .T. ) ;
#12566 = ORIENTED_EDGE ( 'NONE', *, *, #5095, .T. ) ;
#12567 = ORIENTED_EDGE ( 'NONE', *, *, #3564, .T. ) ;
#12568 = VECTOR ( 'NONE', #2515, 1000.000000000000114 ) ;
#12569 = ORIENTED_EDGE ( 'NONE', *, *, #13490, .F. ) ;
#12570 = CARTESIAN_POINT ( 'NONE',  ( 0.000000000000000000, 2.350000000000000089, 0.5149999999999996803 ) ) ;
#12571 = STYLED_ITEM ( 'NONE', ( #10972 ), #9567 ) ;
#12572 = ORIENTED_EDGE ( 'NONE', *, *, #1489, .T. ) ;
#12573 = LINE ( 'NONE', #9237, #1536 ) ;
#12574 = VECTOR ( 'NONE', #6163, 1000.000000000000227 ) ;
#12575 = ORIENTED_EDGE ( 'NONE', *, *, #10049, .F. ) ;
#12576 = LINE ( 'NONE', #2641, #3183 ) ;
#12577 = EDGE_CURVE ( 'NONE', #8845, #7250, #6616, .T. ) ;
#12578 =( NAMED_UNIT ( * ) SI_UNIT ( $, .STERADIAN. ) SOLID_ANGLE_UNIT ( ) );
#12579 = DIRECTION ( 'NONE',  ( 0.000000000000000000, 1.000000000000000000, 0.000000000000000000 ) ) ;
#12580 = AXIS2_PLACEMENT_3D ( 'NONE', #7506, #3315, #3169 ) ;
#12581 = APPLICATION_CONTEXT ( 'automotive_design' ) ;
#12582 = CARTESIAN_POINT ( 'NONE',  ( -302.4999999999999432, -75.00000000000008527, 329.9999999999999432 ) ) ;
#12583 = CARTESIAN_POINT ( 'NONE',  ( 2.740000000000000213, -0.5149999999999973488, -0.6774776749089248540 ) ) ;
#12584 = CARTESIAN_POINT ( 'NONE',  ( 2.740000000000000213, 0.9838866223910001096, 0.5149999999999999023 ) ) ;
#12585 = EDGE_CURVE ( 'NONE', #232, #1387, #9960, .T. ) ;
#12586 = EDGE_LOOP ( 'NONE', ( #3259, #3558, #5857, #3559 ) ) ;
#12587 = CARTESIAN_POINT ( 'NONE',  ( 0.3208286057739604957, -4.433571671609698228, -0.3503314178412692548 ) ) ;
#12588 = LINE ( 'NONE', #13744, #4695 ) ;
#12589 = FACE_OUTER_BOUND ( 'NONE', #7264, .T. ) ;
#12590 = VERTEX_POINT ( 'NONE', #6550 ) ;
#12591 = FACE_OUTER_BOUND ( 'NONE', #4958, .T. ) ;
#12592 = CARTESIAN_POINT ( 'NONE',  ( 352.0000000000000000, 0.000000000000000000, 188.0000000000000000 ) ) ;
#12593 = EDGE_CURVE ( 'NONE', #1600, #7393, #2480, .T. ) ;
#12594 = LINE ( 'NONE', #4919, #5476 ) ;
#12595 = EDGE_LOOP ( 'NONE', ( #3698, #10270 ) ) ;
#12596 = FACE_OUTER_BOUND ( 'NONE', #11392, .T. ) ;
#12597 = CARTESIAN_POINT ( 'NONE',  ( 0.06760930072668799862, 0.5149999999999969047, 0.9010842325122926377 ) ) ;
#12598 = VERTEX_POINT ( 'NONE', #6476 ) ;
#12599 = CARTESIAN_POINT ( 'NONE',  ( -30.00000000000002842, -25.00000000000000000, -169.9999999999999716 ) ) ;
#12600 = EDGE_CURVE ( 'NONE', #2437, #191, #4448, .T. ) ;
#12601 = EDGE_CURVE ( 'NONE', #12519, #6497, #9885, .T. ) ;
#12602 = DIRECTION ( 'NONE',  ( -1.000000000000000000, -0.000000000000000000, -0.000000000000000000 ) ) ;
#12603 =( LENGTH_UNIT ( ) NAMED_UNIT ( * ) SI_UNIT ( .MILLI., .METRE. ) );
#12604 = ADVANCED_FACE ( 'NONE', ( #4516, #3367 ), #10906, .T. ) ;
#12605 = CYLINDRICAL_SURFACE ( 'NONE', #5571, 2.649999999999985700 ) ;
#12606 = CYLINDRICAL_SURFACE ( 'NONE', #11871, 5.000000000000004441 ) ;
#12607 = DIRECTION ( 'NONE',  ( 0.000000000000000000, -1.000000000000000000, 0.000000000000000000 ) ) ;
#12608 = CLOSED_SHELL ( 'NONE', ( #12405, #5859, #7716, #6944, #5407, #6323, #5419, #6509, #4199, #10846 ) ) ;
#12609 = DIRECTION ( 'NONE',  ( -1.000000000000000000, 0.000000000000000000, 0.000000000000000000 ) ) ;
#12610 = ITEM_DEFINED_TRANSFORMATION ( 'NONE', 'NONE', #10022,  #14039 ) ;
#12611 = ORIENTED_EDGE ( 'NONE', *, *, #5607, .F. ) ;
#12612 = VERTEX_POINT ( 'NONE', #2337 ) ;
#12613 = DIRECTION ( 'NONE',  ( 0.000000000000000000, 0.000000000000000000, 1.000000000000000000 ) ) ;
#12614 = ORIENTED_EDGE ( 'NONE', *, *, #4592, .F. ) ;
#12615 = CARTESIAN_POINT ( 'NONE',  ( 4.101954839143203912, -2.368264730583031330, -3.681130640444377988 ) ) ;
#12616 = CARTESIAN_POINT ( 'NONE',  ( 229.9999999999999716, -85.00000000000007105, -250.0009999999999764 ) ) ;
#12617 = CIRCLE ( 'NONE', #11707, 5.000000000000004441 ) ;
#12618 = AXIS2_PLACEMENT_3D ( 'NONE', #1090, #2271, #5609 ) ;
#12619 = ORIENTED_EDGE ( 'NONE', *, *, #12800, .T. ) ;
#12620 = CARTESIAN_POINT ( 'NONE',  ( 2.740000000000000213, -0.9838866223905674557, -0.5150000000000000133 ) ) ;
#12621 = ORIENTED_EDGE ( 'NONE', *, *, #13400, .T. ) ;
#12622 = CARTESIAN_POINT ( 'NONE',  ( -302.3499999999999659, 45.00000000000001421, 30.00000000000000000 ) ) ;
#12623 = DIRECTION ( 'NONE',  ( -1.000000000000000000, 0.000000000000000000, 0.000000000000000000 ) ) ;
#12624 = ORIENTED_EDGE ( 'NONE', *, *, #13192, .T. ) ;
#12625 = CYLINDRICAL_SURFACE ( 'NONE', #7629, 4.749999999999999112 ) ;
#12626 = CARTESIAN_POINT ( 'NONE',  ( 434.9999999999999432, 8.660254037844390851, 199.9990000000000236 ) ) ;
#12627 = APPLICATION_PROTOCOL_DEFINITION ( 'draft international standard', 'automotive_design', 1998, #2114 ) ;
#12628 = CARTESIAN_POINT ( 'NONE',  ( -30.00000000000002842, -225.0000000000000000, 190.0000000000000000 ) ) ;
#12629 = AXIS2_PLACEMENT_3D ( 'NONE', #12758, #10369, #2830 ) ;
#12630 = ORIENTED_EDGE ( 'NONE', *, *, #4368, .T. ) ;
#12631 = ORIENTED_EDGE ( 'NONE', *, *, #705, .F. ) ;
#12632 = ORIENTED_EDGE ( 'NONE', *, *, #11028, .T. ) ;
#12633 = EDGE_CURVE ( 'NONE', #13795, #4174, #9678, .T. ) ;
#12634 = DIRECTION ( 'NONE',  ( 0.000000000000000000, 0.000000000000000000, -1.000000000000000000 ) ) ;
#12635 = ORIENTED_EDGE ( 'NONE', *, *, #13930, .F. ) ;
#12636 = LINE ( 'NONE', #12713, #4792 ) ;
#12637 = EDGE_LOOP ( 'NONE', ( #8739, #13033, #10154, #6134, #9231, #12290, #10983 ) ) ;
#12638 = LINE ( 'NONE', #7273, #13820 ) ;
#12639 = CIRCLE ( 'NONE', #565, 2.041999999999999815 ) ;
#12640 = CYLINDRICAL_SURFACE ( 'NONE', #10630, 5.500000000000005329 ) ;
#12641 = DIRECTION ( 'NONE',  ( -0.000000000000000000, -0.000000000000000000, 1.000000000000000000 ) ) ;
#12642 = CARTESIAN_POINT ( 'NONE',  ( 2.500000000000000000, 2.357898499370431722, -2.818925648462311528E-15 ) ) ;
#12643 = DIRECTION ( 'NONE',  ( 1.000000000000000000, 0.000000000000000000, 0.000000000000000000 ) ) ;
#12644 = DIRECTION ( 'NONE',  ( -1.000000000000000000, 0.000000000000000000, 0.000000000000000000 ) ) ;
#12645 = ORIENTED_EDGE ( 'NONE', *, *, #2447, .T. ) ;
#12646 = ORIENTED_EDGE ( 'NONE', *, *, #12785, .T. ) ;
#12647 = CIRCLE ( 'NONE', #5469, 2.500000000000000000 ) ;
#12648 = EDGE_CURVE ( 'NONE', #2665, #8357, #2954, .T. ) ;
#12649 = CONICAL_SURFACE ( 'NONE', #1290, 5.560781378645573980, 1.221730476396046816 ) ;
#12650 = CARTESIAN_POINT ( 'NONE',  ( 2.500000000000000000, -1.768423874527823569, 1.021000000000002794 ) ) ;
#12651 = LINE ( 'NONE', #10638, #12103 ) ;
#12652 = CARTESIAN_POINT ( 'NONE',  ( -2.500000000000000888, 0.000000000000000000, -4.974599999999998801 ) ) ;
#12653 = AXIS2_PLACEMENT_3D ( 'NONE', #5655, #10079, #13476 ) ;
#12654 = ORIENTED_EDGE ( 'NONE', *, *, #2992, .T. ) ;
#12655 = EDGE_CURVE ( 'NONE', #5183, #1682, #6966, .T. ) ;
#12656 = VECTOR ( 'NONE', #1339, 1000.000000000000000 ) ;
#12657 = VECTOR ( 'NONE', #3041, 1000.000000000000114 ) ;
#12658 = DIRECTION ( 'NONE',  ( 1.000000000000000000, 0.000000000000000000, 0.000000000000000000 ) ) ;
#12659 = ADVANCED_FACE ( 'NONE', ( #1370 ), #7039, .F. ) ;
#12660 = DIRECTION ( 'NONE',  ( 0.8191520442889902442, 1.003171929053522651E-16, -0.5735764363510482688 ) ) ;
#12661 = DIRECTION ( 'NONE',  ( 1.000000000000000000, 0.000000000000000000, 0.000000000000000000 ) ) ;
#12662 = DIRECTION ( 'NONE',  ( -1.000000000000000000, -0.000000000000000000, -0.000000000000000000 ) ) ;
#12663 = CARTESIAN_POINT ( 'NONE',  ( -1.999999999999998668, 1.249139735130300365E-15, 10.20000000000000107 ) ) ;
#12664 = AXIS2_PLACEMENT_3D ( 'NONE', #6187, #8360, #3869 ) ;
#12665 = EDGE_LOOP ( 'NONE', ( #4376, #3094, #9884, #14149 ) ) ;
#12666 = DIRECTION ( 'NONE',  ( -1.000000000000000000, 0.000000000000000000, 0.000000000000000000 ) ) ;
#12667=STYLED_ITEM('',(#14403),#8362);
#12668 = CARTESIAN_POINT ( 'NONE',  ( 1.999999999999998224, 0.000000000000000000, 0.000000000000000000 ) ) ;
#12669 = AXIS2_PLACEMENT_3D ( 'NONE', #5638, #8966, #2516 ) ;
#12670 = VECTOR ( 'NONE', #11194, 1000.000000000000000 ) ;
#12671 = ORIENTED_EDGE ( 'NONE', *, *, #3848, .T. ) ;
#12673 = ADVANCED_FACE ( 'NONE', ( #11467 ), #12480, .F. ) ;
#12672 = LINE ( 'NONE', #3903, #4560 ) ;
#12674 =( NAMED_UNIT ( * ) SI_UNIT ( $, .STERADIAN. ) SOLID_ANGLE_UNIT ( ) );
#12675 = EDGE_CURVE ( 'NONE', #6378, #8377, #9293, .T. ) ;
#12676 = AXIS2_PLACEMENT_3D ( 'NONE', #65, #4525, #207 ) ;
#12677 = SURFACE_SIDE_STYLE ('',( #8320 ) ) ;
#12678 = DIRECTION ( 'NONE',  ( -0.000000000000000000, 0.000000000000000000, 1.000000000000000000 ) ) ;
#12679 =( GEOMETRIC_REPRESENTATION_CONTEXT ( 3 ) GLOBAL_UNCERTAINTY_ASSIGNED_CONTEXT ( ( #1684 ) ) GLOBAL_UNIT_ASSIGNED_CONTEXT ( ( #1589, #1814, #7115 ) ) REPRESENTATION_CONTEXT ( 'NONE', 'WORKASPACE' ) );
#12680 = LINE ( 'NONE', #10436, #4233 ) ;
#12681 = CARTESIAN_POINT ( 'NONE',  ( 79.99999999999971578, 35.00000000000000000, 10.00000000000000000 ) ) ;
#12682 = CONTEXT_DEPENDENT_SHAPE_REPRESENTATION ( #9185, #4167 ) ;
#12683 = CIRCLE ( 'NONE', #12669, 2.500000000000002220 ) ;
#12684 = ORIENTED_EDGE ( 'NONE', *, *, #34, .F. ) ;
#12685 = ADVANCED_FACE ( 'NONE', ( #7107 ), #1305, .F. ) ;
#12686 = FACE_OUTER_BOUND ( 'NONE', #12924, .T. ) ;
#12687 = VERTEX_POINT ( 'NONE', #10448 ) ;
#12688 = CYLINDRICAL_SURFACE ( 'NONE', #10042, 2.649999999999985700 ) ;
#12689 = DIRECTION ( 'NONE',  ( 1.000000000000000000, 0.000000000000000000, 0.000000000000000000 ) ) ;
#12690 = VERTEX_POINT ( 'NONE', #329 ) ;
#12691 = DIRECTION ( 'NONE',  ( 1.000000000000000000, 0.000000000000000000, 0.000000000000000000 ) ) ;
#12692 = EDGE_LOOP ( 'NONE', ( #1289, #6838, #9359 ) ) ;
#12694 = EDGE_CURVE ( 'NONE', #4138, #1971, #5712, .T. ) ;
#12693 = CARTESIAN_POINT ( 'NONE',  ( 2.740000000000000213, 0.6774776749089228556, 0.5149999999999997913 ) ) ;
#12695 = AXIS2_PLACEMENT_3D ( 'NONE', #1026, #2143, #8889 ) ;
#12696 = CARTESIAN_POINT ( 'NONE',  ( 259.0000000000000000, 8.660254037844390851, 200.0000000000000000 ) ) ;
#12697 = ORIENTED_EDGE ( 'NONE', *, *, #1250, .F. ) ;
#12698 = LINE ( 'NONE', #2768, #13835 ) ;
#12699 = CARTESIAN_POINT ( 'NONE',  ( 470.0000000000000000, -25.00000000000000000, 250.0000000000000000 ) ) ;
#12700 = DIRECTION ( 'NONE',  ( 0.000000000000000000, 0.000000000000000000, -1.000000000000000000 ) ) ;
#12701 = PRODUCT_CONTEXT ( 'NONE', #11288, 'mechanical' ) ;
#12702 = DIRECTION ( 'NONE',  ( 1.000000000000000000, 0.000000000000000000, 0.000000000000000000 ) ) ;
#12703 = VERTEX_POINT ( 'NONE', #13629 ) ;
#12704 =( REPRESENTATION_RELATIONSHIP ('NONE','NONE', #11251, #9307 ) REPRESENTATION_RELATIONSHIP_WITH_TRANSFORMATION ( #13621 )SHAPE_REPRESENTATION_RELATIONSHIP( ) );
#12705 = ORIENTED_EDGE ( 'NONE', *, *, #10302, .T. ) ;
#12706 = EDGE_CURVE ( 'NONE', #11791, #5335, #2016, .T. ) ;
#12707 = ORIENTED_EDGE ( 'NONE', *, *, #5092, .F. ) ;
#12708 = EDGE_LOOP ( 'NONE', ( #7950, #858, #11186, #11307 ) ) ;
#12709 = ADVANCED_FACE ( 'NONE', ( #11398 ), #13704, .T. ) ;
#12710 = LINE ( 'NONE', #2783, #5385 ) ;
#12711 = VECTOR ( 'NONE', #13409, 1000.000000000000000 ) ;
#12712 = VERTEX_POINT ( 'NONE', #3705 ) ;
#12713 = CARTESIAN_POINT ( 'NONE',  ( 197.5000000000000000, -90.00000000000007105, 55.00000000000001421 ) ) ;
#12714 = ORIENTED_EDGE ( 'NONE', *, *, #5774, .T. ) ;
#12715 = FACE_BOUND ( 'NONE', #10855, .T. ) ;
#12716 = ADVANCED_FACE ( 'NONE', ( #3566, #4874 ), #10299, .F. ) ;
#12717 = AXIS2_PLACEMENT_3D ( 'NONE', #11109, #2178, #6602 ) ;
#12718 = UNCERTAINTY_MEASURE_WITH_UNIT (LENGTH_MEASURE( 1.000000000000000082E-05 ), #12603, 'distance_accuracy_value', 'NONE');
#12719 = LINE ( 'NONE', #7989, #12017 ) ;
#12720 = CARTESIAN_POINT ( 'NONE',  ( 136.6666666666666288, -20.00000000000000000, -219.8500000000001080 ) ) ;
#12721 = CARTESIAN_POINT ( 'NONE',  ( 0.000000000000000000, 0.000000000000000000, 200.0000000000000000 ) ) ;
#12722 = CARTESIAN_POINT ( 'NONE',  ( 2.500000000000000000, 2.357898499370431722, -2.818925648462311528E-15 ) ) ;
#12723 = DIRECTION ( 'NONE',  ( -0.000000000000000000, 0.000000000000000000, 1.000000000000000000 ) ) ;
#12724 = PRODUCT_DEFINITION_SHAPE ( 'NONE', 'NONE',  #14341 ) ;
#12725 = ORIENTED_EDGE ( 'NONE', *, *, #9241, .F. ) ;
#12726 = EDGE_LOOP ( 'NONE', ( #379, #6792, #10978, #10089 ) ) ;
#12727 = DIRECTION ( 'NONE',  ( 1.000000000000000000, 0.000000000000000000, 0.000000000000000000 ) ) ;
#12728 = CARTESIAN_POINT ( 'NONE',  ( 2.000000000000005329, -3.464101615137751722, 0.000000000000000000 ) ) ;
#12729 = CIRCLE ( 'NONE', #10184, 2.500000000000000444 ) ;
#12730 = CARTESIAN_POINT ( 'NONE',  ( -30.00000000000002842, -225.0000000000000000, 169.9999999999999716 ) ) ;
#12731 =( BOUNDED_SURFACE ( )  B_SPLINE_SURFACE ( 3, 2, ( 
 ( #1869, #760, #5220 ),
 ( #9639, #4129, #8545 ),
 ( #12973, #3046, #6371 ),
 ( #834, #4607, #13245 ),
 ( #1254, #7994, #6787 ),
 ( #3455, #6850, #10803 ) ),
 .UNSPECIFIED., .F., .F., .F. ) 
 B_SPLINE_SURFACE_WITH_KNOTS ( ( 4, 2, 4 ),
 ( 3, 3 ),
 ( 0.02027065861071770947, 0.02273072267836921331, 0.02519078674602071716 ),
 ( 0.000000000000000000, 1.000000000000000000 ),
 .UNSPECIFIED. ) 
 GEOMETRIC_REPRESENTATION_ITEM ( )  RATIONAL_B_SPLINE_SURFACE ( (
 ( 1.000000000000000000, 0.8047781708337304885, 1.000000000000000000),
 ( 1.000000000000000000, 0.8123765190705307671, 1.000000000000000000),
 ( 1.000000000000000000, 0.8190656277163975707, 1.000000000000000000),
 ( 1.000000000000000000, 0.8192366903512159348, 1.000000000000000000),
 ( 1.000000000000000000, 0.8126138454302893610, 1.000000000000000000),
 ( 1.000000000000000000, 0.8047712246031417660, 1.000000000000000000) ) ) 
 REPRESENTATION_ITEM ( '' )  SURFACE ( )  );
#12732 = SURFACE_STYLE_USAGE ( .BOTH. , #8302 ) ;
#12733 = ORIENTED_EDGE ( 'NONE', *, *, #13813, .T. ) ;
#12734 = AXIS2_PLACEMENT_3D ( 'NONE', #6138, #1630, #6071 ) ;
#12735 = DIRECTION ( 'NONE',  ( -0.000000000000000000, -0.000000000000000000, 1.000000000000000000 ) ) ;
#12736 = EDGE_CURVE ( 'NONE', #7342, #6282, #5880, .T. ) ;
#12737 = DIRECTION ( 'NONE',  ( 1.000000000000000000, 0.000000000000000000, 0.000000000000000000 ) ) ;
#12738 = CARTESIAN_POINT ( 'NONE',  ( 439.9999999999999432, 0.000000000000000000, -159.9999999999999716 ) ) ;
#12739 = CARTESIAN_POINT ( 'NONE',  ( 302.6499999999999204, -95.00000000000008527, -190.0000000000000000 ) ) ;
#12740 = DIRECTION ( 'NONE',  ( -0.000000000000000000, -0.000000000000000000, 1.000000000000000000 ) ) ;
#12741 = AXIS2_PLACEMENT_3D ( 'NONE', #6217, #6074, #7018 ) ;
#12742 = ORIENTED_EDGE ( 'NONE', *, *, #16, .T. ) ;
#12743 = CARTESIAN_POINT ( 'NONE',  ( 1.411581201560190495E-15, 4.862606272033091592, -3.745885042887436622 ) ) ;
#12744 = CARTESIAN_POINT ( 'NONE',  ( -1.999999999999996669, 11.05000000000000071, 0.000000000000000000 ) ) ;
#12745 = EDGE_LOOP ( 'NONE', ( #5414, #2921, #5050, #10025 ) ) ;
#12746 = CARTESIAN_POINT ( 'NONE',  ( 119.9999999999999147, -20.00000000000000000, 169.9999999999999716 ) ) ;
#12747 = EDGE_CURVE ( 'NONE', #4602, #13282, #6662, .T. ) ;
#12748 = AXIS2_PLACEMENT_3D ( 'NONE', #3822, #7020, #8234 ) ;
#12749 = CARTESIAN_POINT ( 'NONE',  ( -31.74999999999995737, 0.000000000000000000, 0.000000000000000000 ) ) ;
#12750 = CARTESIAN_POINT ( 'NONE',  ( 2.500000000000000000, 2.500728763858895382E-16, -2.041999999999999815 ) ) ;
#12751 = DIRECTION ( 'NONE',  ( -1.000000000000000000, 0.000000000000000000, 0.000000000000000000 ) ) ;
#12752 = FACE_BOUND ( 'NONE', #1156, .T. ) ;
#12753 = AXIS2_PLACEMENT_3D ( 'NONE', #6879, #9277, #1432 ) ;
#12754 = CARTESIAN_POINT ( 'NONE',  ( -3.522875095019672109, 2.820352903225427532, -3.598441714920591394 ) ) ;
#12755 = ITEM_DEFINED_TRANSFORMATION ( 'NONE', 'NONE', #489,  #14039 ) ;
#12756 = ORIENTED_EDGE ( 'NONE', *, *, #13667, .F. ) ;
#12757 = EDGE_CURVE ( 'NONE', #4789, #5358, #4732, .T. ) ;
#12758 = CARTESIAN_POINT ( 'NONE',  ( 2.500000000000000000, 2.357898499370433054, -1.951563910473907981E-15 ) ) ;
#12759 = EDGE_CURVE ( 'NONE', #10523, #5871, #4798, .T. ) ;
#12760 = AXIS2_PLACEMENT_3D ( 'NONE', #10123, #4617, #8757 ) ;
#12761 = ORIENTED_EDGE ( 'NONE', *, *, #1602, .T. ) ;
#12762 = CARTESIAN_POINT ( 'NONE',  ( 134.9999999999999716, 45.00000000000001421, 0.000000000000000000 ) ) ;
#12763 = LINE ( 'NONE', #10520, #1440 ) ;
#12764 = APPLICATION_CONTEXT ( 'automotive_design' ) ;
#12765 = ORIENTED_EDGE ( 'NONE', *, *, #8262, .T. ) ;
#12766 = DIRECTION ( 'NONE',  ( -0.000000000000000000, 1.000000000000000000, -0.000000000000000000 ) ) ;
#12767 = ORIENTED_EDGE ( 'NONE', *, *, #4268, .T. ) ;
#12768 = AXIS2_PLACEMENT_3D ( 'NONE', #6485, #10772, #8512 ) ;
#12769 = DIRECTION ( 'NONE',  ( 0.000000000000000000, 0.000000000000000000, 1.000000000000000000 ) ) ;
#12770 = DIRECTION ( 'NONE',  ( -0.000000000000000000, -0.000000000000000000, 1.000000000000000000 ) ) ;
#12771 = VERTEX_POINT ( 'NONE', #2623 ) ;
#12772 = UNCERTAINTY_MEASURE_WITH_UNIT (LENGTH_MEASURE( 1.000000000000000082E-05 ), #9225, 'distance_accuracy_value', 'NONE');
#12773 = FACE_BOUND ( 'NONE', #1525, .T. ) ;
#12774 = DIRECTION ( 'NONE',  ( 0.000000000000000000, 0.000000000000000000, -1.000000000000000000 ) ) ;
#12775 =( NAMED_UNIT ( * ) SI_UNIT ( $, .STERADIAN. ) SOLID_ANGLE_UNIT ( ) );
#12776 = AXIS2_PLACEMENT_3D ( 'NONE', #3745, #12735, #12658 ) ;
#12777 = CYLINDRICAL_SURFACE ( 'NONE', #12288, 2.500000000000002220 ) ;
#12778 = APPLICATION_PROTOCOL_DEFINITION ( 'draft international standard', 'automotive_design', 1998, #3418 ) ;
#12779 = CARTESIAN_POINT ( 'NONE',  ( -3.333333333333335258, 2.694301256218251783, -3.300726591567079815 ) ) ;
#12780 = AXIS2_PLACEMENT_3D ( 'NONE', #14264, #10950, #979 ) ;
#12781 = ORIENTED_EDGE ( 'NONE', *, *, #3434, .F. ) ;
#12782 = ORIENTED_EDGE ( 'NONE', *, *, #8333, .T. ) ;
#12783 = EDGE_CURVE ( 'NONE', #8912, #4042, #6824, .T. ) ;
#12784 = DIRECTION ( 'NONE',  ( -1.000000000000000000, -0.000000000000000000, -0.000000000000000000 ) ) ;
#12785 = EDGE_CURVE ( 'NONE', #9136, #6389, #9912, .T. ) ;
#12786 = ORIENTED_EDGE ( 'NONE', *, *, #2960, .F. ) ;
#12787 = CARTESIAN_POINT ( 'NONE',  ( 3.355112389629172576, -2.681727112203168950, -0.2256878752776777242 ) ) ;
#12788 = AXIS2_PLACEMENT_3D ( 'NONE', #6535, #12799, #14214 ) ;
#12789 = VECTOR ( 'NONE', #6307, 1000.000000000000000 ) ;
#12790 = ORIENTED_EDGE ( 'NONE', *, *, #2022, .F. ) ;
#12791 = DIRECTION ( 'NONE',  ( 0.000000000000000000, 0.000000000000000000, 1.000000000000000000 ) ) ;
#12792 = ORIENTED_EDGE ( 'NONE', *, *, #3399, .T. ) ;
#12793 = LINE ( 'NONE', #10471, #1295 ) ;
#12794 = AXIS2_PLACEMENT_3D ( 'NONE', #5348, #14247, #8750 ) ;
#12795 = CYLINDRICAL_SURFACE ( 'NONE', #10595, 13.50000000000000355 ) ;
#12796 = CARTESIAN_POINT ( 'NONE',  ( -294.9999999999999432, 55.00000000000001421, 30.00000000000000000 ) ) ;
#12797 = EDGE_CURVE ( 'NONE', #10304, #10867, #8556, .T. ) ;
#12798 = EDGE_CURVE ( 'NONE', #931, #2006, #13850, .T. ) ;
#12799 = DIRECTION ( 'NONE',  ( -1.000000000000000000, -0.000000000000000000, -0.000000000000000000 ) ) ;
#12800 = EDGE_CURVE ( 'NONE', #258, #6823, #9509, .T. ) ;
#12801 = CARTESIAN_POINT ( 'NONE',  ( 305.4999999999999432, -75.00000000000008527, -190.0000000000000000 ) ) ;
#12802 = FACE_OUTER_BOUND ( 'NONE', #10228, .T. ) ;
#12803 = AXIS2_PLACEMENT_3D ( 'NONE', #10334, #3671, #4840 ) ;
#12804 = ORIENTED_EDGE ( 'NONE', *, *, #3333, .T. ) ;
#12805 = ORIENTED_EDGE ( 'NONE', *, *, #3233, .T. ) ;
#12806 = DIRECTION ( 'NONE',  ( -0.000000000000000000, 1.000000000000000000, -0.000000000000000000 ) ) ;
#12807 = DIRECTION ( 'NONE',  ( 0.000000000000000000, 0.000000000000000000, 1.000000000000000000 ) ) ;
#12808 = EDGE_LOOP ( 'NONE', ( #9408, #5564, #10706, #11644 ) ) ;
#12809 = DIRECTION ( 'NONE',  ( 0.000000000000000000, 1.000000000000000000, 0.000000000000000000 ) ) ;
#12810 = PLANE ( 'NONE',  #6299 ) ;
#12811 = AXIS2_PLACEMENT_3D ( 'NONE', #6203, #7285, #4172 ) ;
#12812 = DIRECTION ( 'NONE',  ( 0.000000000000000000, 0.000000000000000000, -1.000000000000000000 ) ) ;
#12813 = ORIENTED_EDGE ( 'NONE', *, *, #4117, .T. ) ;
#12814 = EDGE_CURVE ( 'NONE', #4081, #5823, #5790, .T. ) ;
#12815 = CARTESIAN_POINT ( 'NONE',  ( 134.5000000000000000, -95.00000000000008527, 190.0000000000000000 ) ) ;
#12816 = DIRECTION ( 'NONE',  ( -0.000000000000000000, -0.000000000000000000, 1.000000000000000000 ) ) ;
#12817 = CARTESIAN_POINT ( 'NONE',  ( 439.9999999999999432, 0.000000000000000000, -169.9999999999999716 ) ) ;
#12818 = DIRECTION ( 'NONE',  ( 0.000000000000000000, 0.000000000000000000, 1.000000000000000000 ) ) ;
#12819 = ORIENTED_EDGE ( 'NONE', *, *, #6119, .F. ) ;
#12820 = CARTESIAN_POINT ( 'NONE',  ( -2.000000000000007550, -3.464101615137749945, 0.000000000000000000 ) ) ;
#12821 = EDGE_CURVE ( 'NONE', #6723, #11371, #9835, .T. ) ;
#12822 = DIRECTION ( 'NONE',  ( 0.000000000000000000, 0.000000000000000000, -1.000000000000000000 ) ) ;
#12823 = VERTEX_POINT ( 'NONE', #4946 ) ;
#12824 = CARTESIAN_POINT ( 'NONE',  ( 82.99999999999998579, 8.660254037844390851, 199.9990000000000236 ) ) ;
#12825 = DIRECTION ( 'NONE',  ( 0.000000000000000000, 0.000000000000000000, -1.000000000000000000 ) ) ;
#12826 = CARTESIAN_POINT ( 'NONE',  ( -1.391697335622809950, -4.043246145443391448, -3.503898532754372575 ) ) ;
#12827 = DIRECTION ( 'NONE',  ( -1.000000000000000000, 0.000000000000000000, 0.000000000000000000 ) ) ;
#12828 = CARTESIAN_POINT ( 'NONE',  ( -4.141042297810615835, 2.227970268150415656, -3.687027686973619822 ) ) ;
#12829 = ITEM_DEFINED_TRANSFORMATION ( 'NONE', 'NONE', #8624,  #14039 ) ;
#12830 = EDGE_LOOP ( 'NONE', ( #4566, #3050 ) ) ;
#12831 = PLANE ( 'NONE',  #7760 ) ;
#12832 = ORIENTED_EDGE ( 'NONE', *, *, #4992, .F. ) ;
#12833 = LINE ( 'NONE', #1806, #12355 ) ;
#12834 = CARTESIAN_POINT ( 'NONE',  ( -25.39999999999996305, 0.000000000000000000, 0.000000000000000000 ) ) ;
#12835 = ORIENTED_EDGE ( 'NONE', *, *, #251, .F. ) ;
#12836 = CARTESIAN_POINT ( 'NONE',  ( 137.4999999999999432, -36.99999999999997868, -169.9999999999999716 ) ) ;
#12837 = VERTEX_POINT ( 'NONE', #9651 ) ;
#12838 = DIRECTION ( 'NONE',  ( -1.000000000000000000, -0.000000000000000000, -0.000000000000000000 ) ) ;
#12839 = CARTESIAN_POINT ( 'NONE',  ( 2.500000000000000000, 0.000000000000000000, 0.000000000000000000 ) ) ;
#12840 = ORIENTED_EDGE ( 'NONE', *, *, #12655, .F. ) ;
#12841 = LINE ( 'NONE', #8194, #11746 ) ;
#12842 = EDGE_CURVE ( 'NONE', #11685, #11973, #1551, .T. ) ;
#12843 = CARTESIAN_POINT ( 'NONE',  ( 4.197393957002303999, 7.772902908466098641E-14, -3.503767560748929810 ) ) ;
#12844 =( LENGTH_UNIT ( ) NAMED_UNIT ( * ) SI_UNIT ( .MILLI., .METRE. ) );
#12845 = ADVANCED_BREP_SHAPE_REPRESENTATION ( '', ( #3574, #14039 ), #7000 ) ;
#12846 = CARTESIAN_POINT ( 'NONE',  ( 142.6500000000000057, -75.00000000000008527, 186.2999999999999829 ) ) ;
#12847 = VERTEX_POINT ( 'NONE', #8263 ) ;
#12848 = ORIENTED_EDGE ( 'NONE', *, *, #12339, .F. ) ;
#12849 = CARTESIAN_POINT ( 'NONE',  ( 144.9999999999999716, -64.99999999999997158, 0.000000000000000000 ) ) ;
#12850 = CLOSED_SHELL ( 'NONE', ( #11017, #1030, #5723, #12257, #9265, #3905, #8971, #966, #1535, #8899, #4698, #8714, #12500, #2510, #10730, #12156, #14260, #618, #11494, #14258, #2900, #5526, #11393, #5326, #9049, #2328, #2502 ) ) ;
#12851 = EDGE_LOOP ( 'NONE', ( #9831, #965, #66, #9210, #10160, #4795 ) ) ;
#12852 = CARTESIAN_POINT ( 'NONE',  ( -2.000000000000001776, 0.000000000000000000, -13.29999999999999893 ) ) ;
#12853 = EDGE_LOOP ( 'NONE', ( #2984, #3902, #2784, #5393, #7783 ) ) ;
#12854 = CARTESIAN_POINT ( 'NONE',  ( 4.999999999999999112, 8.660254037844390851, 210.0000000000000000 ) ) ;
#12855 = VERTEX_POINT ( 'NONE', #8336 ) ;
#12856 = LINE ( 'NONE', #1750, #9435 ) ;
#12857 = CARTESIAN_POINT ( 'NONE',  ( 242.4999999999999716, -80.00000000000007105, 55.00000000000001421 ) ) ;
#12858 = DIRECTION ( 'NONE',  ( 0.000000000000000000, 0.000000000000000000, -1.000000000000000000 ) ) ;
#12859 = EDGE_CURVE ( 'NONE', #5386, #10300, #13147, .T. ) ;
#12860 = AXIS2_PLACEMENT_3D ( 'NONE', #10295, #4793, #12267 ) ;
#12861 = DIRECTION ( 'NONE',  ( 0.000000000000000000, 0.000000000000000000, 1.000000000000000000 ) ) ;
#12862 = CIRCLE ( 'NONE', #6376, 9.999999999999998224 ) ;
#12863 = DIRECTION ( 'NONE',  ( 0.000000000000000000, -1.224646799147353454E-16, 1.000000000000000000 ) ) ;
#12864 = VERTEX_POINT ( 'NONE', #633 ) ;
#12865 = ORIENTED_EDGE ( 'NONE', *, *, #7159, .T. ) ;
#12866 = EDGE_CURVE ( 'NONE', #7321, #9112, #9437, .T. ) ;
#12867 = EDGE_CURVE ( 'NONE', #12771, #9739, #9584, .T. ) ;
#12868 = CARTESIAN_POINT ( 'NONE',  ( -4.000000000000000888, -1.539600717839011201, -3.300726591567081591 ) ) ;
#12869 = AXIS2_PLACEMENT_3D ( 'NONE', #7700, #14228, #11854 ) ;
#12870 = AXIS2_PLACEMENT_3D ( 'NONE', #10277, #305, #10003 ) ;
#12871 = ORIENTED_EDGE ( 'NONE', *, *, #12092, .F. ) ;
#12872 = PLANE ( 'NONE',  #12430 ) ;
#12873 = DIRECTION ( 'NONE',  ( -1.000000000000000000, 0.000000000000000000, 0.000000000000000000 ) ) ;
#12874 = CARTESIAN_POINT ( 'NONE',  ( 140.0000000000000000, -95.00000000000008527, 169.9999999999999716 ) ) ;
#12875 = ORIENTED_EDGE ( 'NONE', *, *, #896, .T. ) ;
#12876 = ADVANCED_FACE ( 'NONE', ( #8408 ), #12911, .T. ) ;
#12877 = CARTESIAN_POINT ( 'NONE',  ( 2.740000000000000213, -0.6774776749089226335, -0.5150000000000000133 ) ) ;
#12878 = CIRCLE ( 'NONE', #2449, 2.500000000000002220 ) ;
#12879 = DIRECTION ( 'NONE',  ( -0.000000000000000000, -0.000000000000000000, 1.000000000000000000 ) ) ;
#12880 = DIRECTION ( 'NONE',  ( -1.000000000000000000, 0.000000000000000000, 6.123233995736766036E-17 ) ) ;
#12881 = PLANE ( 'NONE',  #12734 ) ;
#12882 = AXIS2_PLACEMENT_3D ( 'NONE', #2388, #6291, #9570 ) ;
#12883 = ORIENTED_EDGE ( 'NONE', *, *, #2723, .T. ) ;
#12884 = VERTEX_POINT ( 'NONE', #12836 ) ;
#12885 = EDGE_CURVE ( 'NONE', #10535, #2842, #373, .T. ) ;
#12886 = DIRECTION ( 'NONE',  ( 0.000000000000000000, 0.000000000000000000, 1.000000000000000000 ) ) ;
#12887 = VECTOR ( 'NONE', #12740, 1000.000000000000000 ) ;
#12888 = CARTESIAN_POINT ( 'NONE',  ( 2.500000000000000000, 1.178949249685213863, -2.042000000000001148 ) ) ;
#12889 =( GEOMETRIC_REPRESENTATION_CONTEXT ( 3 ) GLOBAL_UNCERTAINTY_ASSIGNED_CONTEXT ( ( #12718 ) ) GLOBAL_UNIT_ASSIGNED_CONTEXT ( ( #12603, #10580, #313 ) ) REPRESENTATION_CONTEXT ( 'NONE', 'WORKASPACE' ) );
#12890 = AXIS2_PLACEMENT_3D ( 'NONE', #11560, #8431, #10627 ) ;
#12891 = ORIENTED_EDGE ( 'NONE', *, *, #14032, .T. ) ;
#12892 = FACE_OUTER_BOUND ( 'NONE', #4329, .T. ) ;
#12893 = EDGE_CURVE ( 'NONE', #4042, #67, #12918, .T. ) ;
#12894 = VECTOR ( 'NONE', #5682, 1000.000000000000114 ) ;
#12895 = DIRECTION ( 'NONE',  ( -0.000000000000000000, -0.000000000000000000, 1.000000000000000000 ) ) ;
#12896 = DIRECTION ( 'NONE',  ( 0.000000000000000000, 0.000000000000000000, -1.000000000000000000 ) ) ;
#12897 = CARTESIAN_POINT ( 'NONE',  ( 444.9999999999999432, 8.660254037844390851, 199.9990000000000236 ) ) ;
#12898 = VECTOR ( 'NONE', #9279, 1000.000000000000000 ) ;
#12899 = DIRECTION ( 'NONE',  ( -0.000000000000000000, -0.000000000000000000, -1.000000000000000000 ) ) ;
#12900 = CONTEXT_DEPENDENT_SHAPE_REPRESENTATION ( #11422, #3016 ) ;
#12901 = AXIS2_PLACEMENT_3D ( 'NONE', #5461, #9890, #3011 ) ;
#12902 = VERTEX_POINT ( 'NONE', #7320 ) ;
#12903 = AXIS2_PLACEMENT_3D ( 'NONE', #8579, #6404, #6185 ) ;
#12904 = FACE_OUTER_BOUND ( 'NONE', #7490, .T. ) ;
#12905 = CIRCLE ( 'NONE', #2256, 2.055000000000000160 ) ;
#12906 = ORIENTED_EDGE ( 'NONE', *, *, #12094, .T. ) ;
#12907 = PLANE ( 'NONE',  #9343 ) ;
#12908 = DIRECTION ( 'NONE',  ( -0.000000000000000000, -0.000000000000000000, 1.000000000000000000 ) ) ;
#12909 = CIRCLE ( 'NONE', #12456, 4.250000000000000000 ) ;
#12910 = ORIENTED_EDGE ( 'NONE', *, *, #12271, .F. ) ;
#12911 = PLANE ( 'NONE',  #5293 ) ;
#12912 = ORIENTED_EDGE ( 'NONE', *, *, #13545, .T. ) ;
#12913 = CARTESIAN_POINT ( 'NONE',  ( 294.4999999999999432, -95.00000000000008527, -190.0000000000000000 ) ) ;
#12914 = AXIS2_PLACEMENT_3D ( 'NONE', #5652, #4641, #9056 ) ;
#12915 = CARTESIAN_POINT ( 'NONE',  ( 228.6602540378443393, -80.00000000000007105, 170.0000000000000000 ) ) ;
#12916 = ORIENTED_EDGE ( 'NONE', *, *, #9139, .T. ) ;
#12917 = DIRECTION ( 'NONE',  ( 0.8949343913984144638, 0.4461977533474923430, 0.000000000000000000 ) ) ;
#12918 = CIRCLE ( 'NONE', #5051, 2.041999999999999815 ) ;
#12919 = PLANE ( 'NONE',  #7926 ) ;
#12920 = VECTOR ( 'NONE', #12770, 1000.000000000000000 ) ;
#12921 = ADVANCED_FACE ( 'NONE', ( #5096 ), #10675, .F. ) ;
#12922 = CONTEXT_DEPENDENT_SHAPE_REPRESENTATION ( #11846, #5762 ) ;
#12923 = FACE_OUTER_BOUND ( 'NONE', #3347, .T. ) ;
#12924 = EDGE_LOOP ( 'NONE', ( #12477, #4939, #7147 ) ) ;
#12925 = ORIENTED_EDGE ( 'NONE', *, *, #1774, .F. ) ;
#12926 = PLANE ( 'NONE',  #11007 ) ;
#12927 = VECTOR ( 'NONE', #8970, 1000.000000000000000 ) ;
#12928 = EDGE_LOOP ( 'NONE', ( #719, #2986, #4092 ) ) ;
#12929 = DIRECTION ( 'NONE',  ( 0.000000000000000000, 0.4999999999999993339, -0.8660254037844390407 ) ) ;
#12930 = EDGE_LOOP ( 'NONE', ( #6652, #6583, #738, #7282 ) ) ;
#12931 = CIRCLE ( 'NONE', #10620, 7.864440107515625833 ) ;
#12932 = ORIENTED_EDGE ( 'NONE', *, *, #7304, .T. ) ;
#12933 = DIRECTION ( 'NONE',  ( 0.000000000000000000, -0.5000000000000011102, -0.8660254037844379305 ) ) ;
#12934 = VERTEX_POINT ( 'NONE', #1950 ) ;
#12935 = CARTESIAN_POINT ( 'NONE',  ( 7.345657149124338758, 1.312408941150044583, 0.000000000000000000 ) ) ;
#12936 = LINE ( 'NONE', #14012, #365 ) ;
#12937 = DIRECTION ( 'NONE',  ( -0.000000000000000000, -0.000000000000000000, -1.000000000000000000 ) ) ;
#12938 = AXIS2_PLACEMENT_3D ( 'NONE', #11615, #12774, #5021 ) ;
#12939 = CARTESIAN_POINT ( 'NONE',  ( 0.000000000000000000, 0.000000000000000000, 190.0000000000000000 ) ) ;
#12940 = CARTESIAN_POINT ( 'NONE',  ( 4.999999999999999112, -8.660254037844389075, 205.0000000000000284 ) ) ;
#12941 = EDGE_LOOP ( 'NONE', ( #9124, #12475, #6686, #11808, #10899 ) ) ;
#12942 = TOROIDAL_SURFACE ( 'NONE', #9199, 4.000000000000000000, 0.2500000000000000000 ) ;
#12943 = EDGE_LOOP ( 'NONE', ( #9068, #1176, #10591, #715, #5602, #11444, #6251, #3095, #10440, #3890, #7728, #13420 ) ) ;
#12944 = EDGE_CURVE ( 'NONE', #6215, #566, #610, .T. ) ;
#12945 = DIRECTION ( 'NONE',  ( 0.7071067811865502373, 0.000000000000000000, 0.7071067811865447972 ) ) ;
#12946 = EDGE_CURVE ( 'NONE', #13937, #6309, #7397, .T. ) ;
#12947 = DIRECTION ( 'NONE',  ( 1.000000000000000000, 0.000000000000000000, 0.000000000000000000 ) ) ;
#12948 = DIRECTION ( 'NONE',  ( 1.000000000000000000, 0.000000000000000000, 0.000000000000000000 ) ) ;
#12949 = ORIENTED_EDGE ( 'NONE', *, *, #12706, .T. ) ;
#12950 = AXIS2_PLACEMENT_3D ( 'NONE', #2675, #13694, #3770 ) ;
#12951 = LINE ( 'NONE', #9701, #7670 ) ;
#12952 = AXIS2_PLACEMENT_3D ( 'NONE', #13783, #12562, #8195 ) ;
#12953 = EDGE_CURVE ( 'NONE', #11371, #924, #11427, .T. ) ;
#12954 = DIRECTION ( 'NONE',  ( 1.000000000000000000, 0.000000000000000000, 0.000000000000000000 ) ) ;
#12955 = DIRECTION ( 'NONE',  ( 0.000000000000000000, 0.000000000000000000, 1.000000000000000000 ) ) ;
#12956 = DIRECTION ( 'NONE',  ( 0.000000000000000000, 0.000000000000000000, -1.000000000000000000 ) ) ;
#12957 = ORIENTED_EDGE ( 'NONE', *, *, #4791, .T. ) ;
#12958 = EDGE_LOOP ( 'NONE', ( #11479, #8303, #9670, #11465, #6986, #4472, #5966, #13168 ) ) ;
#12959 = AXIS2_PLACEMENT_3D ( 'NONE', #1795, #6228, #13980 ) ;
#12960 = EDGE_CURVE ( 'NONE', #4912, #981, #4620, .T. ) ;
#12961 = FACE_BOUND ( 'NONE', #6046, .T. ) ;
#12962 = ADVANCED_FACE ( 'NONE', ( #10060 ), #3465, .T. ) ;
#12963 = PRODUCT_DEFINITION_SHAPE ( 'NONE', 'NONE',  #14368 ) ;
#12964 = DIRECTION ( 'NONE',  ( -1.000000000000000000, 0.000000000000000000, 0.000000000000000000 ) ) ;
#12965 = ADVANCED_FACE ( 'NONE', ( #846 ), #2493, .T. ) ;
#12966 = VERTEX_POINT ( 'NONE', #12233 ) ;
#12967 = CARTESIAN_POINT ( 'NONE',  ( 0.06760930072668813740, -0.5150000000000026779, 0.9010842325122891960 ) ) ;
#12968 = PRODUCT_DEFINITION_CONTEXT ( 'detailed design', #13774, 'design' ) ;
#12969 = DIRECTION ( 'NONE',  ( -0.000000000000000000, -0.000000000000000000, -1.000000000000000000 ) ) ;
#12970 = VECTOR ( 'NONE', #13091, 1000.000000000000000 ) ;
#12971 = EDGE_CURVE ( 'NONE', #9959, #1020, #6721, .T. ) ;
#12972 = ADVANCED_FACE ( 'NONE', ( #2221, #3533, #6651, #8904, #13316, #10126 ), #89, .T. ) ;
#12973 = CARTESIAN_POINT ( 'NONE',  ( 4.000000000000000000, -0.8732470631449981147, -3.223155494240760088 ) ) ;
#12974 = CARTESIAN_POINT ( 'NONE',  ( 259.0000000000000000, -8.660254037844389075, 205.0000000000000284 ) ) ;
#12975 = DIRECTION ( 'NONE',  ( 0.000000000000000000, 0.000000000000000000, 1.000000000000000000 ) ) ;
#12976 = AXIS2_PLACEMENT_3D ( 'NONE', #5923, #10503, #5073 ) ;
#12977 = EDGE_CURVE ( 'NONE', #9413, #5437, #11296, .T. ) ;
#12978 = ADVANCED_FACE ( 'NONE', ( #6796 ), #3395, .F. ) ;
#12979 = ORIENTED_EDGE ( 'NONE', *, *, #8079, .F. ) ;
#12980 = EDGE_CURVE ( 'NONE', #6984, #10102, #7937, .T. ) ;
#12981 = CARTESIAN_POINT ( 'NONE',  ( 299.9999999999999432, -95.00000000000008527, 186.2999999999999829 ) ) ;
#12982 = EDGE_LOOP ( 'NONE', ( #3805, #10349, #4978, #7812 ) ) ;
#12983 = CARTESIAN_POINT ( 'NONE',  ( 5.560781378645575757, 0.000000000000000000, -4.000000000000000000 ) ) ;
#12984 = DIRECTION ( 'NONE',  ( 0.000000000000000000, 0.000000000000000000, -1.000000000000000000 ) ) ;
#12985 =( REPRESENTATION_RELATIONSHIP ('NONE','NONE', #11251, #2275 ) REPRESENTATION_RELATIONSHIP_WITH_TRANSFORMATION ( #12829 )SHAPE_REPRESENTATION_RELATIONSHIP( ) );
#12986 = AXIS2_PLACEMENT_3D ( 'NONE', #11005, #2565, #1528 ) ;
#12987 = EDGE_LOOP ( 'NONE', ( #8122, #4214, #5308, #2385 ) ) ;
#12988 = CARTESIAN_POINT ( 'NONE',  ( -4.197393957002303999, -7.773935952363655451E-14, -3.503767560748929810 ) ) ;
#12989 = ORIENTED_EDGE ( 'NONE', *, *, #12759, .F. ) ;
#12990 = CARTESIAN_POINT ( 'NONE',  ( 434.9999999999999432, -8.660254037844389075, 205.0000000000000284 ) ) ;
#12991 = CARTESIAN_POINT ( 'NONE',  ( -31.74999999999995737, 0.000000000000000000, 0.000000000000000000 ) ) ;
#12992 = EDGE_LOOP ( 'NONE', ( #14124, #2468, #2415, #422 ) ) ;
#12993 = CARTESIAN_POINT ( 'NONE',  ( 0.000000000000000000, 0.000000000000000000, -200.0000000000000000 ) ) ;
#12994 = VECTOR ( 'NONE', #7886, 1000.000000000000000 ) ;
#12995 = DIRECTION ( 'NONE',  ( -0.000000000000000000, -1.000000000000000000, -0.000000000000000000 ) ) ;
#12996 = LINE ( 'NONE', #2995, #2116 ) ;
#12997 = CARTESIAN_POINT ( 'NONE',  ( 1.734723475976807094E-15, 4.618802153517012954, -0.4999999999999995559 ) ) ;
#12998 = AXIS2_PLACEMENT_3D ( 'NONE', #6649, #157, #2434 ) ;
#12999 = ORIENTED_EDGE ( 'NONE', *, *, #3456, .T. ) ;
#13000 = ORIENTED_EDGE ( 'NONE', *, *, #13714, .T. ) ;
#13001 = DIRECTION ( 'NONE',  ( 0.8949343913984143528, -1.557891129246500526E-15, 0.4461977533474922875 ) ) ;
#13002 = ORIENTED_EDGE ( 'NONE', *, *, #13470, .T. ) ;
#13003 = PRESENTATION_LAYER_ASSIGNMENT (  '', '', ( #12530 ) ) ;
#13004 = LINE ( 'NONE', #8356, #5161 ) ;
#13005 = VERTEX_POINT ( 'NONE', #160 ) ;
#13006 = EDGE_CURVE ( 'NONE', #11206, #13517, #7808, .T. ) ;
#13007 = ORIENTED_EDGE ( 'NONE', *, *, #4638, .F. ) ;
#13008 = DIRECTION ( 'NONE',  ( -0.000000000000000000, -0.000000000000000000, -1.000000000000000000 ) ) ;
#13009 = ORIENTED_EDGE ( 'NONE', *, *, #3061, .T. ) ;
#13010 = CARTESIAN_POINT ( 'NONE',  ( 2.500000000000000000, 1.178949249685212974, -2.042000000000001148 ) ) ;
#13011 = CARTESIAN_POINT ( 'NONE',  ( 82.99999999999998579, 8.660254037844390851, 199.9990000000000236 ) ) ;
#13012 = CYLINDRICAL_SURFACE ( 'NONE', #7580, 2.649999999999985700 ) ;
#13013 = DIRECTION ( 'NONE',  ( 0.000000000000000000, 0.4999999999999990008, -0.8660254037844391517 ) ) ;
#13014 = CARTESIAN_POINT ( 'NONE',  ( 181.0000000000000000, -8.660254037844389075, 205.0000000000000284 ) ) ;
#13015 = ORIENTED_EDGE ( 'NONE', *, *, #7916, .F. ) ;
#13016 = VERTEX_POINT ( 'NONE', #2436 ) ;
#13017 = AXIS2_PLACEMENT_3D ( 'NONE', #11708, #5121, #2179 ) ;
#13018 = CIRCLE ( 'NONE', #6763, 2.500000000000002220 ) ;
#13019 = DIRECTION ( 'NONE',  ( -0.000000000000000000, 1.000000000000000000, -0.000000000000000000 ) ) ;
#13020 = ORIENTED_EDGE ( 'NONE', *, *, #7570, .T. ) ;
#13021 = CARTESIAN_POINT ( 'NONE',  ( -297.4999999999999432, -75.00000000000008527, 10.00000000000000178 ) ) ;
#13022 = CARTESIAN_POINT ( 'NONE',  ( 3.700000000000000178, 3.306546357697853733E-16, -2.700000000000000178 ) ) ;
#13023 = ORIENTED_EDGE ( 'NONE', *, *, #12358, .F. ) ;
#13024 = CIRCLE ( 'NONE', #735, 10.00000000000000000 ) ;
#13025 = CARTESIAN_POINT ( 'NONE',  ( 303.3333333333333144, -20.00000000000000000, 219.8500000000001080 ) ) ;
#13026 = EDGE_CURVE ( 'NONE', #4429, #12042, #13520, .T. ) ;
#13027 = AXIS2_PLACEMENT_3D ( 'NONE', #524, #3442, #7584 ) ;
#13028 = CYLINDRICAL_SURFACE ( 'NONE', #4176, 2.649999999999985700 ) ;
#13029 = DIRECTION ( 'NONE',  ( 0.9237280213470682178, 0.3830490080632377725, 0.000000000000000000 ) ) ;
#13030 = CARTESIAN_POINT ( 'NONE',  ( 2.500000000000000000, 2.357898499370431722, -2.818925648462311528E-15 ) ) ;
#13031 = ADVANCED_BREP_SHAPE_REPRESENTATION ( '', ( #13163, #14039 ), #3056 ) ;
#13032 = ORIENTED_EDGE ( 'NONE', *, *, #9709, .F. ) ;
#13033 = ORIENTED_EDGE ( 'NONE', *, *, #4126, .T. ) ;
#13034 = LINE ( 'NONE', #3036, #13659 ) ;
#13035 = AXIS2_PLACEMENT_3D ( 'NONE', #9830, #14238, #1578 ) ;
#13036 = CARTESIAN_POINT ( 'NONE',  ( -30.00000000000000000, 0.000000000000000000, 205.0000000000000284 ) ) ;
#13037 = ORIENTED_EDGE ( 'NONE', *, *, #8564, .T. ) ;
#13038 = STYLED_ITEM ( 'NONE', ( #12184 ), #6958 ) ;
#13039 = ORIENTED_EDGE ( 'NONE', *, *, #12237, .F. ) ;
#13040 = DIRECTION ( 'NONE',  ( 0.000000000000000000, 0.000000000000000000, -1.000000000000000000 ) ) ;
#13041 = FACE_OUTER_BOUND ( 'NONE', #784, .T. ) ;
#13042 = EDGE_CURVE ( 'NONE', #2872, #10967, #5698, .T. ) ;
#13043 = PRODUCT_DEFINITION ( 'UNKNOWN', '', #3771, #8541 ) ;
#13044 = CARTESIAN_POINT ( 'NONE',  ( 2.500000000000000000, 2.357898499370431722, -2.818925648462311528E-15 ) ) ;
#13045 = DIRECTION ( 'NONE',  ( 0.000000000000000000, 0.000000000000000000, 1.000000000000000000 ) ) ;
#13046 = VECTOR ( 'NONE', #13915, 1000.000000000000000 ) ;
#13047 = APPLICATION_CONTEXT ( 'automotive_design' ) ;
#13048 = ORIENTED_EDGE ( 'NONE', *, *, #2153, .F. ) ;
#13049 = FACE_OUTER_BOUND ( 'NONE', #13349, .T. ) ;
#13050 = ORIENTED_EDGE ( 'NONE', *, *, #11691, .F. ) ;
#13051 = DIRECTION ( 'NONE',  ( 0.000000000000000000, 0.000000000000000000, 1.000000000000000000 ) ) ;
#13052 = DIRECTION ( 'NONE',  ( -0.000000000000000000, -0.000000000000000000, -1.000000000000000000 ) ) ;
#13053 = EDGE_CURVE ( 'NONE', #2464, #5376, #231, .T. ) ;
#13054 = EDGE_CURVE ( 'NONE', #4156, #7984, #12683, .T. ) ;
#13055 = ORIENTED_EDGE ( 'NONE', *, *, #11917, .T. ) ;
#13056 = EDGE_CURVE ( 'NONE', #8612, #3237, #5307, .T. ) ;
#13057 = EDGE_LOOP ( 'NONE', ( #3858, #536, #1458, #3656 ) ) ;
#13058 = FACE_OUTER_BOUND ( 'NONE', #12010, .T. ) ;
#13059 = CARTESIAN_POINT ( 'NONE',  ( -1.999999999999998224, 0.000000000000000000, 0.000000000000000000 ) ) ;
#13060 = ORIENTED_EDGE ( 'NONE', *, *, #9330, .F. ) ;
#13061 = DIRECTION ( 'NONE',  ( 1.000000000000000000, 0.000000000000000000, -0.000000000000000000 ) ) ;
#13062 = DIRECTION ( 'NONE',  ( 1.000000000000000000, 0.000000000000000000, 0.000000000000000000 ) ) ;
#13063 = SHAPE_REPRESENTATION_RELATIONSHIP ( 'NONE' , 'NONE' ,  #4229, #4041 ) ;
#13064 = DIRECTION ( 'NONE',  ( -0.000000000000000000, -0.000000000000000000, -1.000000000000000000 ) ) ;
#13065 = ORIENTED_EDGE ( 'NONE', *, *, #2410, .T. ) ;
#13066 = ORIENTED_EDGE ( 'NONE', *, *, #11011, .T. ) ;
#13067 = LINE ( 'NONE', #11919, #13304 ) ;
#13068 = ORIENTED_EDGE ( 'NONE', *, *, #8265, .F. ) ;
#13069 = CARTESIAN_POINT ( 'NONE',  ( 2.500000000000000000, -2.629050547790028551E-15, -2.041999999999999815 ) ) ;
#13070 = ORIENTED_EDGE ( 'NONE', *, *, #7014, .T. ) ;
#13071 = EDGE_CURVE ( 'NONE', #13211, #14235, #4213, .T. ) ;
#13072 = VERTEX_POINT ( 'NONE', #11087 ) ;
#13073 = DIRECTION ( 'NONE',  ( 1.000000000000000000, 0.000000000000000000, -0.000000000000000000 ) ) ;
#13074 = ORIENTED_EDGE ( 'NONE', *, *, #13487, .T. ) ;
#13075 = CARTESIAN_POINT ( 'NONE',  ( 134.5000000000000000, -75.00000000000008527, -190.0000000000000000 ) ) ;
#13076 = CARTESIAN_POINT ( 'NONE',  ( 238.9999999999999432, -85.00000000000007105, 180.0000000000000000 ) ) ;
#13077 = DIRECTION ( 'NONE',  ( 0.000000000000000000, -0.5000000000000009992, -0.8660254037844380415 ) ) ;
#13078 = DIRECTION ( 'NONE',  ( 0.000000000000000000, 1.224646799147351975E-16, 1.000000000000000000 ) ) ;
#13079 = CARTESIAN_POINT ( 'NONE',  ( -2.000000000000001776, 0.000000000000000000, 0.000000000000000000 ) ) ;
#13080 = PRODUCT_DEFINITION_SHAPE ( 'NONE', 'NONE',  #14334 ) ;
#13081 = VERTEX_POINT ( 'NONE', #5563 ) ;
#13082 = ORIENTED_EDGE ( 'NONE', *, *, #825, .F. ) ;
#13083 = DIRECTION ( 'NONE',  ( -1.000000000000000000, -0.000000000000000000, -0.000000000000000000 ) ) ;
#13084 = EDGE_LOOP ( 'NONE', ( #4460, #7248, #5211, #2091 ) ) ;
#13085 = LINE ( 'NONE', #2945, #6412 ) ;
#13086 = CARTESIAN_POINT ( 'NONE',  ( 124.9999999999999574, -64.99999999999997158, 0.000000000000000000 ) ) ;
#13087 = AXIS2_PLACEMENT_3D ( 'NONE', #1723, #5087, #5158 ) ;
#13088 = FACE_OUTER_BOUND ( 'NONE', #1672, .T. ) ;
#13089 = EDGE_LOOP ( 'NONE', ( #13002, #2922, #7874, #11955 ) ) ;
#13090 = CYLINDRICAL_SURFACE ( 'NONE', #2817, 5.500000000000005329 ) ;
#13091 = DIRECTION ( 'NONE',  ( 0.8571673013836870192, 0.000000000000000000, 0.5150380737757234151 ) ) ;
#13092 = CARTESIAN_POINT ( 'NONE',  ( 2.740000000000000213, 0.000000000000000000, 0.000000000000000000 ) ) ;
#13093 = ADVANCED_FACE ( 'NONE', ( #12589 ), #1085, .T. ) ;
#13094 = ORIENTED_EDGE ( 'NONE', *, *, #4907, .T. ) ;
#13095 = AXIS2_PLACEMENT_3D ( 'NONE', #10696, #9605, #14010 ) ;
#13096 = ORIENTED_EDGE ( 'NONE', *, *, #3563, .F. ) ;
#13097 = CARTESIAN_POINT ( 'NONE',  ( 0.2500000000000002220, 0.000000000000000000, 0.000000000000000000 ) ) ;
#13098 = CARTESIAN_POINT ( 'NONE',  ( -1.999999999999998224, 0.000000000000000000, 0.000000000000000000 ) ) ;
#13099 = ADVANCED_FACE ( 'NONE', ( #1701 ), #4819, .F. ) ;
#13100 = ORIENTED_EDGE ( 'NONE', *, *, #1854, .F. ) ;
#13101 = FACE_OUTER_BOUND ( 'NONE', #10010, .T. ) ;
#13102 = AXIS2_PLACEMENT_3D ( 'NONE', #13146, #5327, #727 ) ;
#13103 = CARTESIAN_POINT ( 'NONE',  ( -6.259644161404860030E-16, -4.618802153517027165, -3.433295621305388234 ) ) ;
#13104 = SHAPE_REPRESENTATION ( 'socket head cap screw_iso_ISO 4762 M5 x 20 - 20N', ( #14039 ), #731 ) ;
#13105 = CARTESIAN_POINT ( 'NONE',  ( -20.63749999999999574, 0.000000000000000000, 0.000000000000000000 ) ) ;
#13106 = CARTESIAN_POINT ( 'NONE',  ( 176.0000000000000000, 0.000000000000000000, -188.0000000000000000 ) ) ;
#13107 = CONTEXT_DEPENDENT_SHAPE_REPRESENTATION ( #9754, #5214 ) ;
#13108 = CIRCLE ( 'NONE', #2937, 5.500000000000005329 ) ;
#13109 = ORIENTED_EDGE ( 'NONE', *, *, #11911, .T. ) ;
#13110 = DIRECTION ( 'NONE',  ( 1.000000000000000000, 0.000000000000000000, -0.000000000000000000 ) ) ;
#13111 = AXIS2_PLACEMENT_3D ( 'NONE', #41, #7881, #12324 ) ;
#13112 = ORIENTED_EDGE ( 'NONE', *, *, #1155, .F. ) ;
#13113 = DIRECTION ( 'NONE',  ( 0.000000000000000000, -0.4999999999999993339, 0.8660254037844390407 ) ) ;
#13114 = CARTESIAN_POINT ( 'NONE',  ( -20.63749999999999574, 0.000000000000000000, 0.000000000000000000 ) ) ;
#13115 = EDGE_CURVE ( 'NONE', #11346, #2351, #5914, .T. ) ;
#13116 = AXIS2_PLACEMENT_3D ( 'NONE', #6632, #9905, #7922 ) ;
#13117 = ADVANCED_FACE ( 'NONE', ( #5061 ), #7071, .F. ) ;
#13118 = EDGE_LOOP ( 'NONE', ( #4168, #1830, #10070, #12406 ) ) ;
#13119 = ORIENTED_EDGE ( 'NONE', *, *, #3065, .T. ) ;
#13120 = DIRECTION ( 'NONE',  ( 1.007709689656716815E-16, 1.153406566473941260E-16, -1.000000000000000000 ) ) ;
#13121 = CARTESIAN_POINT ( 'NONE',  ( -3.540020015735593439, -2.810662092924100630, -3.602146406945814672 ) ) ;
#13122 = VERTEX_POINT ( 'NONE', #10335 ) ;
#13123 = AXIS2_PLACEMENT_3D ( 'NONE', #3619, #3834, #7030 ) ;
#13124 =( NAMED_UNIT ( * ) SI_UNIT ( $, .STERADIAN. ) SOLID_ANGLE_UNIT ( ) );
#13125 = AXIS2_PLACEMENT_3D ( 'NONE', #9036, #7800, #7939 ) ;
#13126 = CYLINDRICAL_SURFACE ( 'NONE', #3343, 9.999999999999996447 ) ;
#13127 = CIRCLE ( 'NONE', #4788, 0.2500000000000002220 ) ;
#13128 = CARTESIAN_POINT ( 'NONE',  ( -144.9999999999999432, 55.00000000000001421, 40.00000000000000000 ) ) ;
#13129 = CARTESIAN_POINT ( 'NONE',  ( 1.424271237134740131, 0.000000000000000000, 0.000000000000000000 ) ) ;
#13130 = ADVANCED_FACE ( 'NONE', ( #13886 ), #592, .T. ) ;
#13131 = CARTESIAN_POINT ( 'NONE',  ( -0.3208286057739654917, 4.433571671609680465, -0.3503314178412548774 ) ) ;
#13132 = CIRCLE ( 'NONE', #11997, 2.649999999999985700 ) ;
#13133 = ORIENTED_EDGE ( 'NONE', *, *, #6343, .T. ) ;
#13134 = MANIFOLD_SOLID_BREP ( 'RecessCore', #3589 ) ;
#13135 = ORIENTED_EDGE ( 'NONE', *, *, #2637, .F. ) ;
#13136 = DIRECTION ( 'NONE',  ( 1.000000000000000000, 0.000000000000000000, 0.000000000000000000 ) ) ;
#13137 = CONICAL_SURFACE ( 'NONE', #1545, 2.500000000000002220, 0.7853981633974521648 ) ;
#13138 = VERTEX_POINT ( 'NONE', #1406 ) ;
#13139 = CARTESIAN_POINT ( 'NONE',  ( 359.9999999999997726, 35.00000000000002842, 0.000000000000000000 ) ) ;
#13140 = ADVANCED_FACE ( 'NONE', ( #5844 ), #3742, .T. ) ;
#13141 = ORIENTED_EDGE ( 'NONE', *, *, #5512, .F. ) ;
#13142 = CIRCLE ( 'NONE', #13823, 2.055000000000000160 ) ;
#13143 = ORIENTED_EDGE ( 'NONE', *, *, #5037, .F. ) ;
#13144 = CYLINDRICAL_SURFACE ( 'NONE', #14286, 5.000000000000004441 ) ;
#13145 = ORIENTED_EDGE ( 'NONE', *, *, #8926, .F. ) ;
#13146 = CARTESIAN_POINT ( 'NONE',  ( -299.9999999999999432, -75.00000000000008527, 329.9999999999999432 ) ) ;
#13147 = CIRCLE ( 'NONE', #12225, 2.649999999999985700 ) ;
#13148 = VECTOR ( 'NONE', #13149, 1000.000000000000000 ) ;
#13149 = DIRECTION ( 'NONE',  ( -0.000000000000000000, -0.000000000000000000, 1.000000000000000000 ) ) ;
#13150 = FACE_OUTER_BOUND ( 'NONE', #1272, .T. ) ;
#13151 = DIRECTION ( 'NONE',  ( 1.000000000000000000, 0.000000000000000000, 0.000000000000000000 ) ) ;
#13152 = CIRCLE ( 'NONE', #10614, 5.500000000000005329 ) ;
#13153 = PLANE ( 'NONE',  #5114 ) ;
#13154 = ADVANCED_FACE ( 'NONE', ( #4762 ), #9175, .F. ) ;
#13155 = CIRCLE ( 'NONE', #3888, 9.999999999999980460 ) ;
#13156 = CARTESIAN_POINT ( 'NONE',  ( -134.9999999999999716, 45.00000000000001421, 40.00000000000000000 ) ) ;
#13157 = ORIENTED_EDGE ( 'NONE', *, *, #4426, .T. ) ;
#13158 = EDGE_CURVE ( 'NONE', #10673, #13397, #12518, .T. ) ;
#13159 = VECTOR ( 'NONE', #11274, 1000.000000000000000 ) ;
#13160 = ORIENTED_EDGE ( 'NONE', *, *, #12353, .T. ) ;
#13161 = EDGE_CURVE ( 'NONE', #14007, #11339, #626, .T. ) ;
#13162 = CARTESIAN_POINT ( 'NONE',  ( 28.70000000000000284, 2.500000000000000000, 0.000000000000000000 ) ) ;
#13163 = MANIFOLD_SOLID_BREP ( 'LPattern1', #5903 ) ;
#13164 = ORIENTED_EDGE ( 'NONE', *, *, #6172, .F. ) ;
#13165 = CARTESIAN_POINT ( 'NONE',  ( 2.500000000000000000, -1.178949249685214307, 2.042000000000001592 ) ) ;
#13166 = DIRECTION ( 'NONE',  ( 1.000000000000000000, 0.000000000000000000, 0.000000000000000000 ) ) ;
#13167 = DIRECTION ( 'NONE',  ( -1.000000000000000000, 0.000000000000000000, 0.000000000000000000 ) ) ;
#13168 = ORIENTED_EDGE ( 'NONE', *, *, #685, .F. ) ;
#13169 = CARTESIAN_POINT ( 'NONE',  ( 145.0000000000000000, 55.00000000000000711, 10.00000000000000000 ) ) ;
#13170 = DIRECTION ( 'NONE',  ( 0.000000000000000000, 0.000000000000000000, -1.000000000000000000 ) ) ;
#13171 = CARTESIAN_POINT ( 'NONE',  ( 0.000000000000000000, 0.000000000000000000, 0.000000000000000000 ) ) ;
#13172 = PRODUCT_DEFINITION_SHAPE ( 'NONE', 'NONE',  #14317 ) ;
#13173 = CARTESIAN_POINT ( 'NONE',  ( 2.740000000000000213, 0.9838866223910003317, 0.5149999999999999023 ) ) ;
#13174 = ORIENTED_EDGE ( 'NONE', *, *, #12004, .T. ) ;
#13175 =( REPRESENTATION_RELATIONSHIP ('NONE','NONE', #11251, #9307 ) REPRESENTATION_RELATIONSHIP_WITH_TRANSFORMATION ( #6448 )SHAPE_REPRESENTATION_RELATIONSHIP( ) );
#13176 = ORIENTED_EDGE ( 'NONE', *, *, #8619, .T. ) ;
#13177 = DIRECTION ( 'NONE',  ( -0.000000000000000000, -0.000000000000000000, 1.000000000000000000 ) ) ;
#13178 = DIRECTION ( 'NONE',  ( 0.000000000000000000, -1.000000000000000000, 0.000000000000000000 ) ) ;
#13179 = VECTOR ( 'NONE', #1871, 1000.000000000000000 ) ;
#13180 = EDGE_CURVE ( 'NONE', #9652, #13843, #3811, .T. ) ;
#13181 = ORIENTED_EDGE ( 'NONE', *, *, #12736, .T. ) ;
#13182 = CARTESIAN_POINT ( 'NONE',  ( 4.999999999999999112, 8.660254037844390851, 200.0000000000000000 ) ) ;
#13183 = DIRECTION ( 'NONE',  ( -0.000000000000000000, -0.000000000000000000, -1.000000000000000000 ) ) ;
#13184 = DIRECTION ( 'NONE',  ( 0.000000000000000000, 0.000000000000000000, -1.000000000000000000 ) ) ;
#13185 = CARTESIAN_POINT ( 'NONE',  ( 53.33333333333330017, -10.00000000000000000, 222.5000000000000853 ) ) ;
#13186 = VECTOR ( 'NONE', #2161, 1000.000000000000000 ) ;
#13187 = EDGE_LOOP ( 'NONE', ( #7692, #2042 ) ) ;
#13188 = FACE_OUTER_BOUND ( 'NONE', #13366, .T. ) ;
#13189 = VERTEX_POINT ( 'NONE', #6496 ) ;
#13190 = DIRECTION ( 'NONE',  ( 1.000000000000000000, 0.000000000000000000, 0.000000000000000000 ) ) ;
#13191 = LINE ( 'NONE', #4210, #4644 ) ;
#13192 = EDGE_CURVE ( 'NONE', #7698, #10043, #12009, .T. ) ;
#13193 = ORIENTED_EDGE ( 'NONE', *, *, #14251, .F. ) ;
#13194 = VERTEX_POINT ( 'NONE', #2949 ) ;
#13195 = CIRCLE ( 'NONE', #6935, 2.649999999999985700 ) ;
#13196 = DIRECTION ( 'NONE',  ( 1.000000000000000000, 0.000000000000000000, 0.000000000000000000 ) ) ;
#13197 = UNCERTAINTY_MEASURE_WITH_UNIT (LENGTH_MEASURE( 1.000000000000000082E-05 ), #9062, 'distance_accuracy_value', 'NONE');
#13198 = PRODUCT_DEFINITION_SHAPE ( 'NONE', 'NONE',  #14349 ) ;
#13199 = DIRECTION ( 'NONE',  ( -1.000000000000000000, 0.000000000000000000, 0.000000000000000000 ) ) ;
#13200 = CARTESIAN_POINT ( 'NONE',  ( -30.00000000000002842, -225.0000000000000000, -190.0000000000000000 ) ) ;
#13201 = DIRECTION ( 'NONE',  ( -0.000000000000000000, -0.000000000000000000, 1.000000000000000000 ) ) ;
#13202 = DIRECTION ( 'NONE',  ( -0.000000000000000000, -0.000000000000000000, -1.000000000000000000 ) ) ;
#13203 = CARTESIAN_POINT ( 'NONE',  ( 305.0000000000000000, -36.99999999999997868, -169.9999999999999716 ) ) ;
#13204 = DIRECTION ( 'NONE',  ( 0.000000000000000000, 0.000000000000000000, -1.000000000000000000 ) ) ;
#13205 = ADVANCED_FACE ( 'NONE', ( #4319, #11942, #6354, #7290, #9834, #9698, #9548, #6275, #5341 ), #4255, .T. ) ;
#13206 = CONTEXT_DEPENDENT_SHAPE_REPRESENTATION ( #11498, #2764 ) ;
#13207 = CARTESIAN_POINT ( 'NONE',  ( -4.203934362469166963, -1.640673743454851286, -3.598432614606932756 ) ) ;
#13208 = EDGE_CURVE ( 'NONE', #1881, #2741, #954, .T. ) ;
#13209 = EDGE_LOOP ( 'NONE', ( #4133, #14224, #3129, #10818 ) ) ;
#13210 = ADVANCED_BREP_SHAPE_REPRESENTATION ( '', ( #13385, #14039 ), #5930 ) ;
#13211 = VERTEX_POINT ( 'NONE', #883 ) ;
#13212 = DIRECTION ( 'NONE',  ( 0.000000000000000000, 0.000000000000000000, 1.000000000000000000 ) ) ;
#13213 = ORIENTED_EDGE ( 'NONE', *, *, #9139, .F. ) ;
#13214 = VECTOR ( 'NONE', #13177, 1000.000000000000000 ) ;
#13215 = LINE ( 'NONE', #9816, #2833 ) ;
#13216 = ORIENTED_EDGE ( 'NONE', *, *, #3333, .F. ) ;
#13217 = ORIENTED_EDGE ( 'NONE', *, *, #11461, .F. ) ;
#13218 = DIRECTION ( 'NONE',  ( -0.7071067811865364705, 0.000000000000000000, 0.7071067811865584529 ) ) ;
#13219 = ORIENTED_EDGE ( 'NONE', *, *, #13390, .F. ) ;
#13220 = AXIS2_PLACEMENT_3D ( 'NONE', #3321, #9717, #2211 ) ;
#13221 = CARTESIAN_POINT ( 'NONE',  ( 242.4999999999999716, -80.00000000000007105, 50.00000000000001421 ) ) ;
#13222 = DIRECTION ( 'NONE',  ( 1.000000000000000000, 0.000000000000000000, 0.000000000000000000 ) ) ;
#13223 = CARTESIAN_POINT ( 'NONE',  ( 222.4999999999999147, -85.00000000000009948, 0.000000000000000000 ) ) ;
#13224 = CARTESIAN_POINT ( 'NONE',  ( 2.500000000000000000, -1.178949249685213863, 2.042000000000002924 ) ) ;
#13225 =( LENGTH_UNIT ( ) NAMED_UNIT ( * ) SI_UNIT ( .MILLI., .METRE. ) );
#13226 = AXIS2_PLACEMENT_3D ( 'NONE', #9710, #754, #10941 ) ;
#13227 = CARTESIAN_POINT ( 'NONE',  ( 203.5000000000000000, -85.00000000000007105, 55.00000000000001421 ) ) ;
#13228 = EDGE_CURVE ( 'NONE', #12687, #3582, #14029, .T. ) ;
#13229 = EDGE_CURVE ( 'NONE', #10176, #5679, #4103, .T. ) ;
#13230 = DIRECTION ( 'NONE',  ( 0.000000000000000000, 0.000000000000000000, -1.000000000000000000 ) ) ;
#13231 = ORIENTED_EDGE ( 'NONE', *, *, #4827, .T. ) ;
#13232 = CIRCLE ( 'NONE', #270, 2.649999999999985700 ) ;
#13233 = ORIENTED_EDGE ( 'NONE', *, *, #9700, .T. ) ;
#13234 = DIRECTION ( 'NONE',  ( 0.000000000000000000, 0.000000000000000000, -1.000000000000000000 ) ) ;
#13235 = CIRCLE ( 'NONE', #3044, 2.500000000000002220 ) ;
#13236 = ORIENTED_EDGE ( 'NONE', *, *, #10206, .T. ) ;
#13237 = PLANE ( 'NONE',  #8490 ) ;
#13238 = CARTESIAN_POINT ( 'NONE',  ( 3.511755186886750923, -2.826662030176382956, -3.597382984111582083 ) ) ;
#13239 = EDGE_CURVE ( 'NONE', #1244, #14268, #2030, .T. ) ;
#13240 = ADVANCED_FACE ( 'NONE', ( #8670, #3024, #7438, #11869, #6207, #812, #8742, #13088 ), #3170, .T. ) ;
#13241 = SURFACE_STYLE_USAGE ( .BOTH. , #3453 ) ;
#13242 = ORIENTED_EDGE ( 'NONE', *, *, #1350, .F. ) ;
#13243 = EDGE_CURVE ( 'NONE', #7848, #2165, #6209, .T. ) ;
#13244 = LINE ( 'NONE', #13169, #13927 ) ;
#13245 = CARTESIAN_POINT ( 'NONE',  ( 4.197310751797292738, 0.8178363989516252985, -3.502498386812444409 ) ) ;
#13246 = CARTESIAN_POINT ( 'NONE',  ( 0.000000000000000000, -0.5149999999999909095, -2.349999999999999201 ) ) ;
#13247 = FACE_BOUND ( 'NONE', #10962, .T. ) ;
#13248 = ORIENTED_EDGE ( 'NONE', *, *, #14160, .T. ) ;
#13249 = FACE_OUTER_BOUND ( 'NONE', #4029, .T. ) ;
#13250 = LINE ( 'NONE', #6794, #1866 ) ;
#13251 = CIRCLE ( 'NONE', #8378, 2.500000000000002220 ) ;
#13252 = CARTESIAN_POINT ( 'NONE',  ( 0.000000000000000000, -0.5149999999999909095, -2.350000000000000977 ) ) ;
#13253 = ORIENTED_EDGE ( 'NONE', *, *, #6736, .F. ) ;
#13254 = DIRECTION ( 'NONE',  ( 1.000000000000000000, 0.000000000000000000, 0.000000000000000000 ) ) ;
#13255 = AXIS2_PLACEMENT_3D ( 'NONE', #4768, #9115, #12380 ) ;
#13256 = AXIS2_PLACEMENT_3D ( 'NONE', #6256, #14084, #8574 ) ;
#13257 = FACE_OUTER_BOUND ( 'NONE', #12987, .T. ) ;
#13258 = DIRECTION ( 'NONE',  ( 0.000000000000000000, 0.000000000000000000, -1.000000000000000000 ) ) ;
#13259 = ITEM_DEFINED_TRANSFORMATION ( 'NONE', 'NONE', #12794,  #14039 ) ;
#13260 = VECTOR ( 'NONE', #8964, 1000.000000000000000 ) ;
#13261 = EDGE_CURVE ( 'NONE', #328, #8099, #7507, .T. ) ;
#13262 = EDGE_LOOP ( 'NONE', ( #7195, #8978 ) ) ;
#13263 = CARTESIAN_POINT ( 'NONE',  ( -1.799999999999996048, 0.000000000000000000, 0.000000000000000000 ) ) ;
#13264 = AXIS2_PLACEMENT_3D ( 'NONE', #10639, #11721, #5275 ) ;
#13265 = ORIENTED_EDGE ( 'NONE', *, *, #9058, .T. ) ;
#13266 = DIRECTION ( 'NONE',  ( 1.000000000000000000, 0.000000000000000000, 0.000000000000000000 ) ) ;
#13267 = EDGE_LOOP ( 'NONE', ( #12786, #2859, #3717, #11146 ) ) ;
#13268 = ORIENTED_EDGE ( 'NONE', *, *, #266, .T. ) ;
#13269 = CARTESIAN_POINT ( 'NONE',  ( 136.6666666666666288, -20.00000000000000000, 219.8500000000001080 ) ) ;
#13270 = CARTESIAN_POINT ( 'NONE',  ( 233.9999999999999432, -85.00000000000007105, 180.0000000000000000 ) ) ;
#13271 = CONICAL_SURFACE ( 'NONE', #11424, 2.500000000000002220, 1.029744260000002631 ) ;
#13272 = SURFACE_STYLE_USAGE ( .BOTH. , #8987 ) ;
#13273 = DIRECTION ( 'NONE',  ( 0.000000000000000000, 0.000000000000000000, -1.000000000000000000 ) ) ;
#13274 = VERTEX_POINT ( 'NONE', #181 ) ;
#13275 = CARTESIAN_POINT ( 'NONE',  ( 0.000000000000000000, 0.000000000000000000, 200.0000000000000000 ) ) ;
#13276 = LINE ( 'NONE', #7685, #9475 ) ;
#13277 = ITEM_DEFINED_TRANSFORMATION ( 'NONE', 'NONE', #1666,  #14039 ) ;
#13278 = CARTESIAN_POINT ( 'NONE',  ( 304.9999999999999432, 45.00000000000001421, 0.000000000000000000 ) ) ;
#13279 = ORIENTED_EDGE ( 'NONE', *, *, #7895, .T. ) ;
#13280 = VERTEX_POINT ( 'NONE', #13440 ) ;
#13281 = FACE_OUTER_BOUND ( 'NONE', #7504, .T. ) ;
#13282 = VERTEX_POINT ( 'NONE', #6846 ) ;
#13283 = CARTESIAN_POINT ( 'NONE',  ( 134.9999999999999716, 45.00000000000001421, -1.230770033143087371E-15 ) ) ;
#13284 = VERTEX_POINT ( 'NONE', #5549 ) ;
#13285 = DIRECTION ( 'NONE',  ( -0.000000000000000000, -0.000000000000000000, 1.000000000000000000 ) ) ;
#13286 = VERTEX_POINT ( 'NONE', #10111 ) ;
#13287 = ADVANCED_FACE ( 'NONE', ( #1324 ), #4536, .F. ) ;
#13288 = DIRECTION ( 'NONE',  ( -0.000000000000000000, 1.000000000000000000, -0.000000000000000000 ) ) ;
#13289 = PRODUCT_DEFINITION_SHAPE ( 'NONE', 'NONE',  #14328 ) ;
#13290 = CARTESIAN_POINT ( 'NONE',  ( 4.000000000000000000, -1.084202172485504434E-14, -3.142992957459231906 ) ) ;
#13291 = SURFACE_STYLE_FILL_AREA ( #9078 ) ;
#13292 = DIRECTION ( 'NONE',  ( 0.000000000000000000, 0.5000000000000012212, 0.8660254037844380415 ) ) ;
#13293 = PLANE ( 'NONE',  #13830 ) ;
#13294 = ORIENTED_EDGE ( 'NONE', *, *, #14212, .T. ) ;
#13295 = ORIENTED_EDGE ( 'NONE', *, *, #12953, .T. ) ;
#13296 = DIRECTION ( 'NONE',  ( -0.000000000000000000, -0.000000000000000000, 1.000000000000000000 ) ) ;
#13297 = ORIENTED_EDGE ( 'NONE', *, *, #1613, .F. ) ;
#13298 = FACE_OUTER_BOUND ( 'NONE', #4149, .T. ) ;
#13299 = EDGE_CURVE ( 'NONE', #4498, #13983, #9981, .T. ) ;
#13300 = FACE_BOUND ( 'NONE', #13262, .T. ) ;
#13301 = PRODUCT_RELATED_PRODUCT_CATEGORY ( 'part', '', ( #3459 ) ) ;
#13302 = DIRECTION ( 'NONE',  ( -0.000000000000000000, -0.000000000000000000, -1.000000000000000000 ) ) ;
#13303 = ORIENTED_EDGE ( 'NONE', *, *, #12241, .F. ) ;
#13304 = VECTOR ( 'NONE', #6610, 1000.000000000000000 ) ;
#13305 = DIRECTION ( 'NONE',  ( 0.000000000000000000, 0.000000000000000000, 1.000000000000000000 ) ) ;
#13306 = CARTESIAN_POINT ( 'NONE',  ( 2.500000000000000000, -2.357898499370432166, 3.035766082959412415E-15 ) ) ;
#13307 = CARTESIAN_POINT ( 'NONE',  ( 3.900000000000000799, 0.000000000000000000, 2.500000000000000000 ) ) ;
#13308 = CARTESIAN_POINT ( 'NONE',  ( 134.9999999999999432, -56.99999999999997158, 0.000000000000000000 ) ) ;
#13309 = EDGE_CURVE ( 'NONE', #1103, #6825, #12931, .T. ) ;
#13310 = EDGE_CURVE ( 'NONE', #12386, #9564, #7648, .T. ) ;
#13311 = ORIENTED_EDGE ( 'NONE', *, *, #3219, .F. ) ;
#13312 = AXIS2_PLACEMENT_3D ( 'NONE', #7486, #859, #3363 ) ;
#13313 = APPLICATION_CONTEXT ( 'automotive_design' ) ;
#13314 = DIRECTION ( 'NONE',  ( -1.000000000000000000, 0.000000000000000000, 0.000000000000000000 ) ) ;
#13315 = ADVANCED_FACE ( 'NONE', ( #10997 ), #864, .T. ) ;
#13316 = FACE_BOUND ( 'NONE', #352, .T. ) ;
#13317 = ORIENTED_EDGE ( 'NONE', *, *, #12885, .T. ) ;
#13318 = DIRECTION ( 'NONE',  ( 0.000000000000000000, 0.000000000000000000, 1.000000000000000000 ) ) ;
#13319 = CARTESIAN_POINT ( 'NONE',  ( -30.00000000000002842, -25.00000000000000000, 190.0000000000000000 ) ) ;
#13320 = LINE ( 'NONE', #11157, #3246 ) ;
#13321 = DIRECTION ( 'NONE',  ( 6.123233995736766036E-17, -1.000000000000000000, 0.000000000000000000 ) ) ;
#13322 = EDGE_CURVE ( 'NONE', #1452, #12590, #1801, .T. ) ;
#13323 = ADVANCED_FACE ( 'NONE', ( #6782 ), #10183, .F. ) ;
#13324 = ORIENTED_EDGE ( 'NONE', *, *, #8590, .T. ) ;
#13325 = CARTESIAN_POINT ( 'NONE',  ( 145.5000000000000284, -75.00000000000008527, 190.0000000000000000 ) ) ;
#13326 = ORIENTED_EDGE ( 'NONE', *, *, #14111, .T. ) ;
#13327 = LINE ( 'NONE', #11165, #4188 ) ;
#13328 = EDGE_CURVE ( 'NONE', #11341, #9866, #13369, .T. ) ;
#13329 = ORIENTED_EDGE ( 'NONE', *, *, #11922, .T. ) ;
#13330 = ORIENTED_EDGE ( 'NONE', *, *, #7635, .F. ) ;
#13331 = LINE ( 'NONE', #6599, #11496 ) ;
#13332 = LINE ( 'NONE', #7679, #13565 ) ;
#13333 = DIRECTION ( 'NONE',  ( 0.000000000000000000, 0.000000000000000000, -1.000000000000000000 ) ) ;
#13334 = CARTESIAN_POINT ( 'NONE',  ( 119.9999999999999147, -225.0010000000000048, 19.99999999999998934 ) ) ;
#13335 = CARTESIAN_POINT ( 'NONE',  ( 0.000000000000000000, 0.000000000000000000, -186.0000000000000000 ) ) ;
#13336 = CARTESIAN_POINT ( 'NONE',  ( 2.740000000000000213, 0.000000000000000000, 0.000000000000000000 ) ) ;
#13337 = FACE_OUTER_BOUND ( 'NONE', #7675, .T. ) ;
#13338 = ITEM_DEFINED_TRANSFORMATION ( 'NONE', 'NONE', #9553,  #14039 ) ;
#13339 = DIRECTION ( 'NONE',  ( 1.000000000000000000, 0.000000000000000000, 0.000000000000000000 ) ) ;
#13340 = AXIS2_PLACEMENT_3D ( 'NONE', #5883, #3783, #331 ) ;
#13341 = ORIENTED_EDGE ( 'NONE', *, *, #1761, .T. ) ;
#13342 = ORIENTED_EDGE ( 'NONE', *, *, #9106, .T. ) ;
#13343 = CARTESIAN_POINT ( 'NONE',  ( 2.740000000000000213, 0.6774776749089226335, -0.5150000000000000133 ) ) ;
#13344 = VERTEX_POINT ( 'NONE', #11211 ) ;
#13345 = CARTESIAN_POINT ( 'NONE',  ( -30.00000000000002842, -15.00000000000000000, 240.0000000000000284 ) ) ;
#13346 = AXIS2_PLACEMENT_3D ( 'NONE', #8567, #11040, #8857 ) ;
#13347 = EDGE_LOOP ( 'NONE', ( #12080, #7477, #4298, #3223 ) ) ;
#13348 = FACE_BOUND ( 'NONE', #4195, .T. ) ;
#13349 = EDGE_LOOP ( 'NONE', ( #14239, #2192, #7186, #2278, #9292 ) ) ;
#13350 = CARTESIAN_POINT ( 'NONE',  ( 386.6666666666666288, -20.00000000000000000, -222.5000000000000853 ) ) ;
#13351 = AXIS2_PLACEMENT_3D ( 'NONE', #11488, #11636, #8363 ) ;
#13352 = CARTESIAN_POINT ( 'NONE',  ( 259.0000000000000000, -8.660254037844389075, 199.9990000000000236 ) ) ;
#13353 = DIRECTION ( 'NONE',  ( 0.000000000000000000, -3.612465276695121047E-15, 1.000000000000000000 ) ) ;
#13354 = EDGE_CURVE ( 'NONE', #4498, #3293, #6449, .T. ) ;
#13355 = DIRECTION ( 'NONE',  ( -0.000000000000000000, -0.000000000000000000, 1.000000000000000000 ) ) ;
#13356 =( NAMED_UNIT ( * ) SI_UNIT ( $, .STERADIAN. ) SOLID_ANGLE_UNIT ( ) );
#13357 = CARTESIAN_POINT ( 'NONE',  ( 197.5000000000000000, -90.00000000000007105, 55.00000000000001421 ) ) ;
#13358 = DIRECTION ( 'NONE',  ( 0.000000000000000000, 0.000000000000000000, 1.000000000000000000 ) ) ;
#13359 = AXIS2_PLACEMENT_3D ( 'NONE', #655, #13944, #7198 ) ;
#13360 = EDGE_LOOP ( 'NONE', ( #9583, #13742, #403, #13756, #8423, #11164, #13557, #6573 ) ) ;
#13361 = VERTEX_POINT ( 'NONE', #5474 ) ;
#13362 = MECHANICAL_DESIGN_GEOMETRIC_PRESENTATION_REPRESENTATION (  '', ( #12667 ), #12679 ) ;
#13364 = PLANE ( 'NONE',  #3769 ) ;
#13363 = VECTOR ( 'NONE', #1532, 1000.000000000000000 ) ;
#13365 = AXIS2_PLACEMENT_3D ( 'NONE', #8799, #8727, #2124 ) ;
#13366 = EDGE_LOOP ( 'NONE', ( #11271, #3812, #9087, #5367 ) ) ;
#13367 = CARTESIAN_POINT ( 'NONE',  ( 319.9999999999999432, -20.00000000000000000, 169.9999999999999716 ) ) ;
#13368 = CARTESIAN_POINT ( 'NONE',  ( 0.000000000000000000, -1.178949249685213863, 2.042000000000002924 ) ) ;
#13369 = LINE ( 'NONE', #6571, #13159 ) ;
#13370 = CIRCLE ( 'NONE', #11287, 10.00000000000000000 ) ;
#13371 = AXIS2_PLACEMENT_3D ( 'NONE', #105, #12255, #2317 ) ;
#13372 = PLANE ( 'NONE',  #4676 ) ;
#13373 = FACE_OUTER_BOUND ( 'NONE', #11459, .T. ) ;
#13374 = AXIS2_PLACEMENT_3D ( 'NONE', #8155, #6062, #9473 ) ;
#13375 = CARTESIAN_POINT ( 'NONE',  ( 53.33333333333330017, -15.00000000000000000, 219.8500000000001080 ) ) ;
#13376 = CARTESIAN_POINT ( 'NONE',  ( 2.100000000000000089, 0.000000000000000000, -4.694516984716113228 ) ) ;
#13377 = EDGE_CURVE ( 'NONE', #5974, #4659, #6676, .T. ) ;
#13378 = EDGE_LOOP ( 'NONE', ( #6041, #521, #13236, #629 ) ) ;
#13379 = EDGE_CURVE ( 'NONE', #9474, #2746, #2207, .T. ) ;
#13380 = LINE ( 'NONE', #9990, #9536 ) ;
#13381 = CARTESIAN_POINT ( 'NONE',  ( -124.9999999999999432, -105.0000000000000853, 40.00000000000000000 ) ) ;
#13382 = AXIS2_PLACEMENT_3D ( 'NONE', #2357, #3244, #7854 ) ;
#13383 = CARTESIAN_POINT ( 'NONE',  ( 4.000000000000000000, 2.309401076758497151, -5.000000000000000000 ) ) ;
#13384 = ORIENTED_EDGE ( 'NONE', *, *, #13261, .F. ) ;
#13385 = MANIFOLD_SOLID_BREP ( 'Boss-Extrude2', #5663 ) ;
#13386 = FACE_OUTER_BOUND ( 'NONE', #4744, .T. ) ;
#13387 = DIRECTION ( 'NONE',  ( 1.000000000000000000, -0.000000000000000000, -0.000000000000000000 ) ) ;
#13388 = DIRECTION ( 'NONE',  ( 0.000000000000000000, 0.000000000000000000, 1.000000000000000000 ) ) ;
#13389 = EDGE_CURVE ( 'NONE', #7620, #8297, #5063, .T. ) ;
#13390 = EDGE_CURVE ( 'NONE', #9074, #7429, #1685, .T. ) ;
#13391 = ORIENTED_EDGE ( 'NONE', *, *, #3925, .T. ) ;
#13392 = VECTOR ( 'NONE', #10804, 1000.000000000000000 ) ;
#13393 = CARTESIAN_POINT ( 'NONE',  ( 359.9999999999997726, 35.00000000000002842, 10.00000000000000000 ) ) ;
#13394 = PRODUCT ( 'roller', 'roller', '', ( #1739 ) ) ;
#13395 = VERTEX_POINT ( 'NONE', #2788 ) ;
#13396 = DIRECTION ( 'NONE',  ( 1.000000000000000000, 0.000000000000000000, 0.000000000000000000 ) ) ;
#13397 = VERTEX_POINT ( 'NONE', #3726 ) ;
#13398 = ORIENTED_EDGE ( 'NONE', *, *, #665, .T. ) ;
#13399 = CARTESIAN_POINT ( 'NONE',  ( 0.2500000000000002220, 5.204748896376250699E-16, -4.250000000000000000 ) ) ;
#13400 = EDGE_CURVE ( 'NONE', #12140, #1151, #2571, .T. ) ;
#13401 = EDGE_CURVE ( 'NONE', #7342, #8845, #7364, .T. ) ;
#13402 = FACE_OUTER_BOUND ( 'NONE', #7371, .T. ) ;
#13403 = EDGE_CURVE ( 'NONE', #1625, #8017, #1392, .T. ) ;
#13404 = AXIS2_PLACEMENT_3D ( 'NONE', #7367, #10567, #12954 ) ;
#13405 = CARTESIAN_POINT ( 'NONE',  ( -996.9834933385058093, 0.000000000000000000, 0.000000000000000000 ) ) ;
#13406 = LINE ( 'NONE', #7955, #11627 ) ;
#13407 = LINE ( 'NONE', #5722, #5264 ) ;
#13408 = SURFACE_STYLE_USAGE ( .BOTH. , #2251 ) ;
#13409 = DIRECTION ( 'NONE',  ( -1.000000000000000000, 0.000000000000000000, 0.000000000000000000 ) ) ;
#13410 = ITEM_DEFINED_TRANSFORMATION ( 'NONE', 'NONE', #7687,  #14039 ) ;
#13411 = VERTEX_POINT ( 'NONE', #4825 ) ;
#13412 = MANIFOLD_SOLID_BREP ( 'M5 Machine Threads Stud1', #2200 ) ;
#13413 = ORIENTED_EDGE ( 'NONE', *, *, #7963, .F. ) ;
#13414 = CARTESIAN_POINT ( 'NONE',  ( 242.5000000000000000, -90.00000000000007105, 50.00000000000001421 ) ) ;
#13415 = EDGE_LOOP ( 'NONE', ( #6835, #7533, #3632, #11908 ) ) ;
#13416 = CYLINDRICAL_SURFACE ( 'NONE', #12109, 2.500000000000002220 ) ;
#13417 = AXIS2_PLACEMENT_3D ( 'NONE', #14107, #12879, #523 ) ;
#13418 = ORIENTED_EDGE ( 'NONE', *, *, #13071, .T. ) ;
#13419 = CARTESIAN_POINT ( 'NONE',  ( 20.00000000000000000, 2.449293598294706513E-15, 190.0000000000000000 ) ) ;
#13420 = ORIENTED_EDGE ( 'NONE', *, *, #2616, .T. ) ;
#13421 = CIRCLE ( 'NONE', #8086, 5.000000000000004441 ) ;
#13422 = CARTESIAN_POINT ( 'NONE',  ( 12.00000000000000000, 1.469576158976823947E-15, 190.0000000000000000 ) ) ;
#13423 = LINE ( 'NONE', #10985, #14287 ) ;
#13424 = CARTESIAN_POINT ( 'NONE',  ( 219.9999999999999716, -25.00000000000000000, 225.1500000000000625 ) ) ;
#13425 = DIRECTION ( 'NONE',  ( -0.000000000000000000, 1.000000000000000000, -0.000000000000000000 ) ) ;
#13426 = PLANE ( 'NONE',  #13889 ) ;
#13427 = PRODUCT_CONTEXT ( 'NONE', #3148, 'mechanical' ) ;
#13428 = FACE_BOUND ( 'NONE', #4170, .T. ) ;
#13429 = EDGE_LOOP ( 'NONE', ( #2640, #2567, #2133, #3859 ) ) ;
#13430 = VECTOR ( 'NONE', #5356, 1000.000000000000114 ) ;
#13431 = AXIS2_PLACEMENT_3D ( 'NONE', #10569, #7446, #12818 ) ;
#13432 = ORIENTED_EDGE ( 'NONE', *, *, #5877, .F. ) ;
#13433 = AXIS2_PLACEMENT_3D ( 'NONE', #5104, #8415, #562 ) ;
#13434 = ORIENTED_EDGE ( 'NONE', *, *, #10798, .T. ) ;
#13435 = EDGE_CURVE ( 'NONE', #634, #5319, #11487, .T. ) ;
#13436 = CARTESIAN_POINT ( 'NONE',  ( 0.7826237921249276086, 0.000000000000000000, 12.44999999999999929 ) ) ;
#13437 = EDGE_LOOP ( 'NONE', ( #14296, #8223, #11137, #3368, #10794 ) ) ;
#13438 = CARTESIAN_POINT ( 'NONE',  ( 144.9999999999999716, -64.99999999999997158, 0.000000000000000000 ) ) ;
#13439 = CARTESIAN_POINT ( 'NONE',  ( 0.000000000000000000, 0.000000000000000000, -190.0000000000000000 ) ) ;
#13440 = CARTESIAN_POINT ( 'NONE',  ( 136.6666666666666288, -25.00000000000000000, 219.8500000000001080 ) ) ;
#13441 = VECTOR ( 'NONE', #176, 1000.000000000000000 ) ;
#13442 =( REPRESENTATION_RELATIONSHIP ('NONE','NONE', #11251, #208 ) REPRESENTATION_RELATIONSHIP_WITH_TRANSFORMATION ( #13410 )SHAPE_REPRESENTATION_RELATIONSHIP( ) );
#13443 = CYLINDRICAL_SURFACE ( 'NONE', #12310, 12.44999999999999929 ) ;
#13444 = CIRCLE ( 'NONE', #14139, 1.050000000000000488 ) ;
#13445 = CYLINDRICAL_SURFACE ( 'NONE', #11835, 5.000000000000004441 ) ;
#13446 = CARTESIAN_POINT ( 'NONE',  ( -124.9999999999999432, -65.00000000000008527, 40.00000000000000000 ) ) ;
#13447 = DIRECTION ( 'NONE',  ( -1.000000000000000000, -0.000000000000000000, -0.000000000000000000 ) ) ;
#13448 = ORIENTED_EDGE ( 'NONE', *, *, #1299, .F. ) ;
#13449 = EDGE_CURVE ( 'NONE', #10366, #10615, #8140, .T. ) ;
#13450 = AXIS2_PLACEMENT_3D ( 'NONE', #13949, #14232, #4164 ) ;
#13451 = DIRECTION ( 'NONE',  ( -0.000000000000000000, -0.000000000000000000, 1.000000000000000000 ) ) ;
#13452 = CARTESIAN_POINT ( 'NONE',  ( 4.000000000000000000, 2.309401076758515803, -0.4999999999999995559 ) ) ;
#13453 = DIRECTION ( 'NONE',  ( 0.8571673013836870192, 0.000000000000000000, 0.5150380737757234151 ) ) ;
#13454 = ORIENTED_EDGE ( 'NONE', *, *, #9935, .T. ) ;
#13455 = ADVANCED_FACE ( 'NONE', ( #11348 ), #9465, .T. ) ;
#13456 = DIRECTION ( 'NONE',  ( -1.000000000000000000, -0.000000000000000000, -0.000000000000000000 ) ) ;
#13457 = PRESENTATION_LAYER_ASSIGNMENT (  '', '', ( #6988 ) ) ;
#13458 = DIRECTION ( 'NONE',  ( 0.000000000000000000, 0.000000000000000000, -1.000000000000000000 ) ) ;
#13459 = DIRECTION ( 'NONE',  ( 6.123233995736766036E-17, -1.000000000000000000, 0.000000000000000000 ) ) ;
#13460 = CONTEXT_DEPENDENT_SHAPE_REPRESENTATION ( #3090, #8560 ) ;
#13461 = VERTEX_POINT ( 'NONE', #4751 ) ;
#13462 = EDGE_LOOP ( 'NONE', ( #11853, #6770, #4313, #7741, #10606, #9559, #4397 ) ) ;
#13463 = AXIS2_PLACEMENT_3D ( 'NONE', #11966, #4059, #13986 ) ;
#13464 = CARTESIAN_POINT ( 'NONE',  ( 3.436319922986518449, -2.634841920959471562, -3.531542292954761741 ) ) ;
#13465 = AXIS2_PLACEMENT_3D ( 'NONE', #3645, #11337, #4325 ) ;
#13466 = EDGE_LOOP ( 'NONE', ( #1499, #7573, #8252, #3239 ) ) ;
#13467 = EDGE_LOOP ( 'NONE', ( #3704, #6017, #3136, #5788 ) ) ;
#13468 = AXIS2_PLACEMENT_3D ( 'NONE', #11774, #10691, #6182 ) ;
#13470 = EDGE_CURVE ( 'NONE', #4582, #3164, #8764, .T. ) ;
#13469 = FACE_OUTER_BOUND ( 'NONE', #12160, .T. ) ;
#13471 = PRODUCT_RELATED_PRODUCT_CATEGORY ( 'part', '', ( #10055 ) ) ;
#13472 = DIRECTION ( 'NONE',  ( -0.000000000000000000, -0.000000000000000000, -1.000000000000000000 ) ) ;
#13473 = PLANE ( 'NONE',  #4360 ) ;
#13474 = LINE ( 'NONE', #8103, #10438 ) ;
#13475 = FACE_OUTER_BOUND ( 'NONE', #11340, .T. ) ;
#13476 = DIRECTION ( 'NONE',  ( 1.000000000000000000, 0.000000000000000000, 0.000000000000000000 ) ) ;
#13477 =( NAMED_UNIT ( * ) PLANE_ANGLE_UNIT ( ) SI_UNIT ( $, .RADIAN. ) );
#13478 = VECTOR ( 'NONE', #13672, 1000.000000000000000 ) ;
#13479 = LINE ( 'NONE', #1497, #5312 ) ;
#13480 = ITEM_DEFINED_TRANSFORMATION ( 'NONE', 'NONE', #12331,  #14039 ) ;
#13481 = AXIS2_PLACEMENT_3D ( 'NONE', #10274, #8011, #166 ) ;
#13482 = ORIENTED_EDGE ( 'NONE', *, *, #1252, .F. ) ;
#13483 = MECHANICAL_DESIGN_GEOMETRIC_PRESENTATION_REPRESENTATION (  '', ( #4003 ), #491 ) ;
#13484 = VECTOR ( 'NONE', #12552, 1000.000000000000000 ) ;
#13485 = ORIENTED_EDGE ( 'NONE', *, *, #7618, .F. ) ;
#13486 = ADVANCED_FACE ( 'NONE', ( #10397 ), #12640, .F. ) ;
#13487 = EDGE_CURVE ( 'NONE', #11362, #1098, #1093, .T. ) ;
#13488 = LINE ( 'NONE', #3560, #10784 ) ;
#13489 = ORIENTED_EDGE ( 'NONE', *, *, #10879, .F. ) ;
#13490 = EDGE_CURVE ( 'NONE', #6568, #3844, #507, .T. ) ;
#13491 = PLANE ( 'NONE',  #7704 ) ;
#13492 = AXIS2_PLACEMENT_3D ( 'NONE', #6705, #4530, #7850 ) ;
#13493 = ORIENTED_EDGE ( 'NONE', *, *, #6032, .T. ) ;
#13494 = DIRECTION ( 'NONE',  ( 0.000000000000000000, 0.000000000000000000, 1.000000000000000000 ) ) ;
#13495 = ORIENTED_EDGE ( 'NONE', *, *, #8891, .T. ) ;
#13496 = CARTESIAN_POINT ( 'NONE',  ( -299.9999999999999432, -75.00000000000008527, 0.000000000000000000 ) ) ;
#13497 = AXIS2_PLACEMENT_3D ( 'NONE', #13171, #10243, #132 ) ;
#13498 = CARTESIAN_POINT ( 'NONE',  ( 2.500000000000000000, 0.000000000000000000, 2.041999999999999815 ) ) ;
#13499 = CARTESIAN_POINT ( 'NONE',  ( -134.9999999999999716, 45.00000000000001421, 40.00000000000000000 ) ) ;
#13500 = CARTESIAN_POINT ( 'NONE',  ( 214.9999999999999716, -85.00000000000007105, 0.000000000000000000 ) ) ;
#13501 = DIRECTION ( 'NONE',  ( -0.000000000000000000, -0.000000000000000000, 1.000000000000000000 ) ) ;
#13502 = ORIENTED_EDGE ( 'NONE', *, *, #8167, .T. ) ;
#13503 = VERTEX_POINT ( 'NONE', #13511 ) ;
#13504 = EDGE_CURVE ( 'NONE', #13543, #12061, #12719, .T. ) ;
#13505 = ORIENTED_EDGE ( 'NONE', *, *, #7562, .T. ) ;
#13506 = DIRECTION ( 'NONE',  ( 1.000000000000000000, 0.000000000000000000, 0.000000000000000000 ) ) ;
#13507 = ORIENTED_EDGE ( 'NONE', *, *, #14193, .T. ) ;
#13508 = LINE ( 'NONE', #866, #4338 ) ;
#13509 = VERTEX_POINT ( 'NONE', #6191 ) ;
#13510 = CARTESIAN_POINT ( 'NONE',  ( 269.0000000000000000, 8.660254037844390851, 205.0000000000000284 ) ) ;
#13511 = CARTESIAN_POINT ( 'NONE',  ( 82.99999999999998579, 8.660254037844390851, 200.0000000000000000 ) ) ;
#13512 = CARTESIAN_POINT ( 'NONE',  ( 469.9999999999998863, -225.0000000000000000, 169.9999999999999716 ) ) ;
#13513 = DIRECTION ( 'NONE',  ( 0.000000000000000000, -0.5000000000000012212, -0.8660254037844380415 ) ) ;
#13514 = DIRECTION ( 'NONE',  ( 1.000000000000000000, 0.000000000000000000, 0.000000000000000000 ) ) ;
#13515 = PRODUCT_DEFINITION_SHAPE ( 'NONE', 'NONE',  #14323 ) ;
#13516 = DIRECTION ( 'NONE',  ( -1.000000000000000000, 0.000000000000000000, 0.000000000000000000 ) ) ;
#13517 = VERTEX_POINT ( 'NONE', #6480 ) ;
#13518 = CARTESIAN_POINT ( 'NONE',  ( 299.9999999999999432, -95.00000000000008527, 190.0000000000000000 ) ) ;
#13519 = LINE ( 'NONE', #9110, #485 ) ;
#13520 = LINE ( 'NONE', #9111, #10608 ) ;
#13521 = ORIENTED_EDGE ( 'NONE', *, *, #10729, .T. ) ;
#13522 = CARTESIAN_POINT ( 'NONE',  ( -31.74999999999995737, 0.000000000000000000, 0.000000000000000000 ) ) ;
#13523 = EDGE_CURVE ( 'NONE', #13895, #5183, #14157, .T. ) ;
#13524 = CARTESIAN_POINT ( 'NONE',  ( 219.9999999999999716, -20.00000000000000000, -225.1500000000000625 ) ) ;
#13525 = DIRECTION ( 'NONE',  ( 0.000000000000000000, 0.000000000000000000, 1.000000000000000000 ) ) ;
#13526 = ORIENTED_EDGE ( 'NONE', *, *, #12338, .F. ) ;
#13527 = CARTESIAN_POINT ( 'NONE',  ( 0.6666666666666689611, 4.233901974057261874, -3.300726591567082480 ) ) ;
#13528 = ORIENTED_EDGE ( 'NONE', *, *, #13666, .T. ) ;
#13529 = CARTESIAN_POINT ( 'NONE',  ( 0.5469614295415388128, -4.303013824935362663, -3.535263753543555598 ) ) ;
#13530 = ORIENTED_EDGE ( 'NONE', *, *, #5626, .T. ) ;
#13531 = VERTEX_POINT ( 'NONE', #13076 ) ;
#13532 = PLANE ( 'NONE',  #13562 ) ;
#13533 = CARTESIAN_POINT ( 'NONE',  ( 2.500000000000000000, -1.178949249685213863, 2.042000000000002924 ) ) ;
#13534 = VECTOR ( 'NONE', #3429, 1000.000000000000000 ) ;
#13535 = AXIS2_PLACEMENT_3D ( 'NONE', #63, #9893, #1450 ) ;
#13536 = CARTESIAN_POINT ( 'NONE',  ( -13.50000000000000000, 1.653273178848926867E-15, 190.0000000000000000 ) ) ;
#13537 = CARTESIAN_POINT ( 'NONE',  ( 7.345657149124971141, -1.312408941149200814, 2.762944903268657774E-16 ) ) ;
#13538 = CYLINDRICAL_SURFACE ( 'NONE', #3525, 2.649999999999985700 ) ;
#13539 = CARTESIAN_POINT ( 'NONE',  ( 145.5000000000000284, -95.00000000000008527, 186.2999999999999829 ) ) ;
#13540 = PRESENTATION_STYLE_ASSIGNMENT (( #4862 ) ) ;
#13541 = CARTESIAN_POINT ( 'NONE',  ( 5.384454397937118664, 0.000000000000000000, -4.484454397937119197 ) ) ;
#13542 = AXIS2_PLACEMENT_3D ( 'NONE', #6464, #7681, #4289 ) ;
#13543 = VERTEX_POINT ( 'NONE', #3159 ) ;
#13544 = ORIENTED_EDGE ( 'NONE', *, *, #4743, .F. ) ;
#13545 = EDGE_CURVE ( 'NONE', #13274, #10393, #7597, .T. ) ;
#13546 = LINE ( 'NONE', #192, #6374 ) ;
#13547 = CIRCLE ( 'NONE', #11957, 7.864440107515430434 ) ;
#13548 = EDGE_CURVE ( 'NONE', #6979, #8753, #869, .T. ) ;
#13549 = ORIENTED_EDGE ( 'NONE', *, *, #3576, .F. ) ;
#13550 = AXIS2_PLACEMENT_3D ( 'NONE', #8767, #1943, #3267 ) ;
#13551 = CARTESIAN_POINT ( 'NONE',  ( 2.500000000000000000, 2.357898499370433054, -1.951563910473907981E-15 ) ) ;
#13552 = VERTEX_POINT ( 'NONE', #7346 ) ;
#13553 = DIRECTION ( 'NONE',  ( 0.000000000000000000, 0.000000000000000000, 1.000000000000000000 ) ) ;
#13554 = ORIENTED_EDGE ( 'NONE', *, *, #12512, .F. ) ;
#13555 = DIRECTION ( 'NONE',  ( 2.478176394252579538E-17, -1.000000000000000000, 0.000000000000000000 ) ) ;
#13556 = DIRECTION ( 'NONE',  ( 0.000000000000000000, -1.000000000000000000, 0.000000000000000000 ) ) ;
#13557 = ORIENTED_EDGE ( 'NONE', *, *, #11196, .F. ) ;
#13558 = B_SPLINE_CURVE_WITH_KNOTS ( 'NONE', 3,
 ( #12249, #4425, #6806, #11099, #11233, #3348 ),
 .UNSPECIFIED., .F., .F.,
 ( 4, 2, 4 ),
 ( 0.003358874760055550156, 0.004541967308452096383, 0.005725059856848641743 ),
 .UNSPECIFIED. ) ;
#13559 =( NAMED_UNIT ( * ) PLANE_ANGLE_UNIT ( ) SI_UNIT ( $, .RADIAN. ) );
#13560 = EDGE_CURVE ( 'NONE', #4926, #6823, #14093, .T. ) ;
#13561 = CARTESIAN_POINT ( 'NONE',  ( 0.000000000000000000, -1.178949249685218303, -2.041999999999998039 ) ) ;
#13562 = AXIS2_PLACEMENT_3D ( 'NONE', #2603, #8237, #4715 ) ;
#13563 =( NAMED_UNIT ( * ) PLANE_ANGLE_UNIT ( ) SI_UNIT ( $, .RADIAN. ) );
#13564 = APPLICATION_PROTOCOL_DEFINITION ( 'draft international standard', 'automotive_design', 1998, #1632 ) ;
#13565 = VECTOR ( 'NONE', #5441, 1000.000000000000000 ) ;
#13566 = CARTESIAN_POINT ( 'NONE',  ( 0.000000000000000000, 0.000000000000000000, 200.0000000000000000 ) ) ;
#13567 = VERTEX_POINT ( 'NONE', #797 ) ;
#13568 = EDGE_CURVE ( 'NONE', #4587, #4579, #4086, .T. ) ;
#13569 = ORIENTED_EDGE ( 'NONE', *, *, #1056, .F. ) ;
#13570 = AXIS2_PLACEMENT_3D ( 'NONE', #13819, #13680, #6682 ) ;
#13571 = VERTEX_POINT ( 'NONE', #3948 ) ;
#13572 = LINE ( 'NONE', #3651, #10433 ) ;
#13573 = VECTOR ( 'NONE', #5862, 1000.000000000000000 ) ;
#13574 = ORIENTED_EDGE ( 'NONE', *, *, #7635, .T. ) ;
#13575 = LINE ( 'NONE', #283, #11739 ) ;
#13576 = ORIENTED_EDGE ( 'NONE', *, *, #7991, .T. ) ;
#13577 = LINE ( 'NONE', #3657, #5717 ) ;
#13578 = CIRCLE ( 'NONE', #587, 4.556291390728477886 ) ;
#13579 = CARTESIAN_POINT ( 'NONE',  ( 3.999999999999999112, -0.7890432684750902093, -0.04868663549882291247 ) ) ;
#13580 = EDGE_CURVE ( 'NONE', #13983, #3594, #4112, .T. ) ;
#13581 = ADVANCED_FACE ( 'NONE', ( #9751 ), #4162, .F. ) ;
#13582 = AXIS2_PLACEMENT_3D ( 'NONE', #10512, #13692, #3694 ) ;
#13583 = CARTESIAN_POINT ( 'NONE',  ( -299.9999999999999432, -75.00000000000008527, 339.9999999999999432 ) ) ;
#13584 = ADVANCED_FACE ( 'NONE', ( #9681 ), #6345, .T. ) ;
#13585 = ADVANCED_FACE ( 'NONE', ( #5195 ), #12795, .T. ) ;
#13586 = PRESENTATION_STYLE_ASSIGNMENT (( #9167 ) ) ;
#13587 = AXIS2_PLACEMENT_3D ( 'NONE', #5669, #127, #1453 ) ;
#13588 = DIRECTION ( 'NONE',  ( 0.000000000000000000, 0.000000000000000000, -1.000000000000000000 ) ) ;
#13589 = DIRECTION ( 'NONE',  ( 1.000000000000000000, 0.000000000000000000, 0.000000000000000000 ) ) ;
#13590 = EDGE_CURVE ( 'NONE', #2924, #7600, #12936, .T. ) ;
#13591 = VECTOR ( 'NONE', #7627, 1000.000000000000000 ) ;
#13592 = EDGE_LOOP ( 'NONE', ( #2548, #13039, #13341, #1744, #10758 ) ) ;
#13593 = VECTOR ( 'NONE', #3010, 1000.000000000000000 ) ;
#13594 = SURFACE_STYLE_FILL_AREA ( #227 ) ;
#13595 = CIRCLE ( 'NONE', #11521, 12.00000000000000000 ) ;
#13596 = DIRECTION ( 'NONE',  ( 1.000000000000000000, 0.000000000000000000, 0.000000000000000000 ) ) ;
#13597 = DIRECTION ( 'NONE',  ( -0.000000000000000000, 0.000000000000000000, 1.000000000000000000 ) ) ;
#13598 = PRESENTATION_LAYER_ASSIGNMENT (  '', '', ( #7806 ) ) ;
#13599 = ORIENTED_EDGE ( 'NONE', *, *, #3527, .T. ) ;
#13600 = AXIS2_PLACEMENT_3D ( 'NONE', #9034, #12308, #11151 ) ;
#13601 = AXIS2_PLACEMENT_3D ( 'NONE', #12991, #8561, #8481 ) ;
#13602 = DIRECTION ( 'NONE',  ( 0.4461977533473793778, -2.936240938438015166E-15, 0.8949343913984707521 ) ) ;
#13603 = DIRECTION ( 'NONE',  ( 0.000000000000000000, 0.000000000000000000, -1.000000000000000000 ) ) ;
#13604 = DIRECTION ( 'NONE',  ( 0.000000000000000000, 0.000000000000000000, 1.000000000000000000 ) ) ;
#13605 = DIRECTION ( 'NONE',  ( 0.000000000000000000, 0.000000000000000000, -1.000000000000000000 ) ) ;
#13606 = ORIENTED_EDGE ( 'NONE', *, *, #5202, .F. ) ;
#13607=STYLED_ITEM('',(#14403),#13385);
#13608 = CARTESIAN_POINT ( 'NONE',  ( 140.0000000000000000, -95.00000000000008527, 186.2999999999999829 ) ) ;
#13609 = EDGE_CURVE ( 'NONE', #3237, #13622, #7425, .T. ) ;
#13610 = FACE_OUTER_BOUND ( 'NONE', #13961, .T. ) ;
#13611 = ORIENTED_EDGE ( 'NONE', *, *, #2022, .T. ) ;
#13612 = ORIENTED_EDGE ( 'NONE', *, *, #2334, .F. ) ;
#13613 = FACE_BOUND ( 'NONE', #10198, .T. ) ;
#13614 = CARTESIAN_POINT ( 'NONE',  ( 444.9999999999999432, -8.660254037844389075, 199.9990000000000236 ) ) ;
#13615 = LINE ( 'NONE', #4857, #2939 ) ;
#13616 = DIRECTION ( 'NONE',  ( 0.000000000000000000, -0.000000000000000000, -1.000000000000000000 ) ) ;
#13617 = CARTESIAN_POINT ( 'NONE',  ( -4.000000000000000000, -2.309401076758512694, -3.433295621305382461 ) ) ;
#13618 = CARTESIAN_POINT ( 'NONE',  ( 0.000000000000000000, 15.00000000000000000, 205.0000000000000284 ) ) ;
#13619 = AXIS2_PLACEMENT_3D ( 'NONE', #6851, #12299, #5688 ) ;
#13620 = CARTESIAN_POINT ( 'NONE',  ( -1.999999999999998668, 0.000000000000000000, -10.20000000000000107 ) ) ;
#13621 = ITEM_DEFINED_TRANSFORMATION ( 'NONE', 'NONE', #3085,  #14039 ) ;
#13622 = VERTEX_POINT ( 'NONE', #4240 ) ;
#13623 = ORIENTED_EDGE ( 'NONE', *, *, #11830, .F. ) ;
#13624 = DIRECTION ( 'NONE',  ( -0.000000000000000000, 1.000000000000000000, -0.000000000000000000 ) ) ;
#13625 = EDGE_CURVE ( 'NONE', #3306, #9712, #12905, .T. ) ;
#13626 = ORIENTED_EDGE ( 'NONE', *, *, #9596, .T. ) ;
#13627 = CARTESIAN_POINT ( 'NONE',  ( 386.6666666666666288, -25.00000000000000000, 222.5000000000000853 ) ) ;
#13628 = ORIENTED_EDGE ( 'NONE', *, *, #9973, .F. ) ;
#13629 = CARTESIAN_POINT ( 'NONE',  ( 229.9999999999999432, -85.00000000000007105, 170.0000000000000000 ) ) ;
#13630 = ORIENTED_EDGE ( 'NONE', *, *, #12018, .F. ) ;
#13631 = VECTOR ( 'NONE', #11959, 1000.000000000000114 ) ;
#13632 = DIRECTION ( 'NONE',  ( 0.000000000000000000, 0.000000000000000000, -1.000000000000000000 ) ) ;
#13633 = PRODUCT_DEFINITION_SHAPE ( 'NONE', 'NONE',  #14319 ) ;
#13634 = DIRECTION ( 'NONE',  ( -1.000000000000000000, 0.000000000000000000, 0.000000000000000000 ) ) ;
#13635 = ORIENTED_EDGE ( 'NONE', *, *, #1177, .F. ) ;
#13636 = SURFACE_STYLE_USAGE ( .BOTH. , #10528 ) ;
#13637 = EDGE_CURVE ( 'NONE', #2602, #4143, #11931, .T. ) ;
#13638 = CARTESIAN_POINT ( 'NONE',  ( 3.700000000000000178, 0.000000000000000000, 2.700000000000000178 ) ) ;
#13639 =( LENGTH_UNIT ( ) NAMED_UNIT ( * ) SI_UNIT ( .MILLI., .METRE. ) );
#13640 = DIRECTION ( 'NONE',  ( 1.000000000000000000, 0.000000000000000000, 0.000000000000000000 ) ) ;
#13641 = ITEM_DEFINED_TRANSFORMATION ( 'NONE', 'NONE', #11866,  #14039 ) ;
#13642 = CARTESIAN_POINT ( 'NONE',  ( 299.9999999999999432, -75.00000000000008527, 186.2999999999999829 ) ) ;
#13643 = ORIENTED_EDGE ( 'NONE', *, *, #9018, .T. ) ;
#13644 = TOROIDAL_SURFACE ( 'NONE', #9729, 10.20000000000000107, 0.2000000000000031197 ) ;
#13645 = ORIENTED_EDGE ( 'NONE', *, *, #12279, .T. ) ;
#13646 = ORIENTED_EDGE ( 'NONE', *, *, #4556, .F. ) ;
#13647 = CARTESIAN_POINT ( 'NONE',  ( 219.9999999999999716, -85.00000000000007105, 190.0000000000000000 ) ) ;
#13648 = VECTOR ( 'NONE', #11334, 1000.000000000000000 ) ;
#13649 = ORIENTED_EDGE ( 'NONE', *, *, #11962, .T. ) ;
#13650 = DIRECTION ( 'NONE',  ( -0.000000000000000000, -0.000000000000000000, 1.000000000000000000 ) ) ;
#13651 = VERTEX_POINT ( 'NONE', #8658 ) ;
#13652 = DIRECTION ( 'NONE',  ( 1.000000000000000000, 0.000000000000000000, -0.000000000000000000 ) ) ;
#13653 = DIRECTION ( 'NONE',  ( -0.000000000000000000, -0.000000000000000000, 1.000000000000000000 ) ) ;
#13654 = DIRECTION ( 'NONE',  ( -0.000000000000000000, 1.000000000000000000, -0.000000000000000000 ) ) ;
#13655 = VECTOR ( 'NONE', #13736, 1000.000000000000000 ) ;
#13656 = EDGE_CURVE ( 'NONE', #9120, #9740, #5328, .T. ) ;
#13657 = PRODUCT_DEFINITION ( 'UNKNOWN', '', #6320, #829 ) ;
#13658 = DIRECTION ( 'NONE',  ( 1.000000000000000000, 0.000000000000000000, 0.000000000000000000 ) ) ;
#13659 = VECTOR ( 'NONE', #7590, 1000.000000000000000 ) ;
#13660 = VECTOR ( 'NONE', #11800, 1000.000000000000000 ) ;
#13661 =( LENGTH_UNIT ( ) NAMED_UNIT ( * ) SI_UNIT ( .MILLI., .METRE. ) );
#13662 = CARTESIAN_POINT ( 'NONE',  ( 1.849560077140141701, -0.5149999999999969047, -0.7556913915602436749 ) ) ;
#13663 = PRESENTATION_LAYER_ASSIGNMENT (  '', '', ( #672 ) ) ;
#13664 = PLANE ( 'NONE',  #5677 ) ;
#13665 = ORIENTED_EDGE ( 'NONE', *, *, #10052, .F. ) ;
#13666 = EDGE_CURVE ( 'NONE', #1682, #7893, #1752, .T. ) ;
#13667 = EDGE_CURVE ( 'NONE', #2677, #11323, #9535, .T. ) ;
#13668 = SHAPE_REPRESENTATION_RELATIONSHIP ( 'NONE' , 'NONE' ,  #3832, #1760 ) ;
#13669 = AXIS2_PLACEMENT_3D ( 'NONE', #8828, #12155, #13506 ) ;
#13670 = EDGE_CURVE ( 'NONE', #7167, #7113, #10129, .T. ) ;
#13671 = CARTESIAN_POINT ( 'NONE',  ( 132.4999999999999432, -56.99999999999997158, -169.9999999999999716 ) ) ;
#13672 = DIRECTION ( 'NONE',  ( -1.000000000000000000, -0.000000000000000000, -0.000000000000000000 ) ) ;
#13673 =( LENGTH_UNIT ( ) NAMED_UNIT ( * ) SI_UNIT ( .MILLI., .METRE. ) );
#13674 = ORIENTED_EDGE ( 'NONE', *, *, #2672, .F. ) ;
#13675 = CIRCLE ( 'NONE', #7873, 2.649999999999985700 ) ;
#13676 = DIRECTION ( 'NONE',  ( 0.000000000000000000, 0.000000000000000000, 1.000000000000000000 ) ) ;
#13677 = CARTESIAN_POINT ( 'NONE',  ( 1.794155980045909482, 5.265981236333621429E-16, -4.300000000000001599 ) ) ;
#13678 = DIRECTION ( 'NONE',  ( 1.000000000000000000, 0.000000000000000000, 0.000000000000000000 ) ) ;
#13679 = CIRCLE ( 'NONE', #11602, 2.100000000000000089 ) ;
#13680 = DIRECTION ( 'NONE',  ( -1.000000000000000000, 0.000000000000000000, -0.000000000000000000 ) ) ;
#13681 = AXIS2_PLACEMENT_3D ( 'NONE', #1468, #11784, #13078 ) ;
#13682 = ORIENTED_EDGE ( 'NONE', *, *, #1880, .T. ) ;
#13683 = CARTESIAN_POINT ( 'NONE',  ( -124.9999999999999432, -105.0000000000000853, 30.00000000000000000 ) ) ;
#13684 = DIRECTION ( 'NONE',  ( -1.000000000000000000, 0.000000000000000000, -0.000000000000000000 ) ) ;
#13685 = VECTOR ( 'NONE', #597, 1000.000000000000000 ) ;
#13686 = ORIENTED_EDGE ( 'NONE', *, *, #9415, .F. ) ;
#13687 = DIRECTION ( 'NONE',  ( -0.000000000000000000, -0.000000000000000000, -1.000000000000000000 ) ) ;
#13688 = PLANE ( 'NONE',  #3614 ) ;
#13689 = DIRECTION ( 'NONE',  ( -0.000000000000000000, -0.000000000000000000, 1.000000000000000000 ) ) ;
#13690 = FACE_OUTER_BOUND ( 'NONE', #9369, .T. ) ;
#13691 = CARTESIAN_POINT ( 'NONE',  ( -2.855764796983342624, 2.970025579236414082, -0.09382832055445475272 ) ) ;
#13692 = DIRECTION ( 'NONE',  ( -0.000000000000000000, -0.000000000000000000, 1.000000000000000000 ) ) ;
#13693 = ADVANCED_FACE ( 'NONE', ( #4306 ), #12069, .T. ) ;
#13694 = DIRECTION ( 'NONE',  ( -0.000000000000000000, -0.000000000000000000, 1.000000000000000000 ) ) ;
#13695 = CIRCLE ( 'NONE', #7452, 2.041999999999999815 ) ;
#13696 = ORIENTED_EDGE ( 'NONE', *, *, #5751, .F. ) ;
#13697 = VERTEX_POINT ( 'NONE', #7904 ) ;
#13698 = DIRECTION ( 'NONE',  ( 1.000000000000000000, 0.000000000000000000, 0.000000000000000000 ) ) ;
#13699 =( GEOMETRIC_REPRESENTATION_CONTEXT ( 3 ) GLOBAL_UNCERTAINTY_ASSIGNED_CONTEXT ( ( #11613 ) ) GLOBAL_UNIT_ASSIGNED_CONTEXT ( ( #6373, #6298, #762 ) ) REPRESENTATION_CONTEXT ( 'NONE', 'WORKASPACE' ) );
#13700 = ORIENTED_EDGE ( 'NONE', *, *, #2360, .F. ) ;
#13701 = CARTESIAN_POINT ( 'NONE',  ( 434.9999999999999432, 8.660254037844390851, 199.9990000000000236 ) ) ;
#13702 = CARTESIAN_POINT ( 'NONE',  ( 140.0000000000000000, -95.00000000000008527, 169.9999999999999716 ) ) ;
#13703 = ORIENTED_EDGE ( 'NONE', *, *, #4554, .F. ) ;
#13704 = PLANE ( 'NONE',  #11996 ) ;
#13705 = EDGE_LOOP ( 'NONE', ( #5860, #11879, #10882, #7143, #12399, #11391, #10239, #11048, #4843, #9745, #1059, #6181, #175 ) ) ;
#13706 = CARTESIAN_POINT ( 'NONE',  ( 3.016506661494197328, 7.007546303702493782E-17, 0.000000000000000000 ) ) ;
#13707 = DIRECTION ( 'NONE',  ( -0.8571673013836870192, 0.000000000000000000, -0.5150380737757234151 ) ) ;
#13709 = VERTEX_POINT ( 'NONE', #5604 ) ;
#13708 = CONICAL_SURFACE ( 'NONE', #2145, 4.000000000000000000, 0.8911886515913786111 ) ;
#13710 = PLANE ( 'NONE',  #4571 ) ;
#13711 = CARTESIAN_POINT ( 'NONE',  ( -3.264624719419710521E-13, -4.796980096169328966, -3.721999068284310486 ) ) ;
#13712 = AXIS2_PLACEMENT_3D ( 'NONE', #2885, #749, #4185 ) ;
#13713 = COLOUR_RGB ( '',0.8941176470588234615, 0.8941176470588234615, 0.8941176470588234615 ) ;
#13714 = EDGE_CURVE ( 'NONE', #6820, #4205, #12346, .T. ) ;
#13715 = DIRECTION ( 'NONE',  ( 0.000000000000000000, -0.000000000000000000, 1.000000000000000000 ) ) ;
#13716 = APPLICATION_PROTOCOL_DEFINITION ( 'draft international standard', 'automotive_design', 1998, #11288 ) ;
#13717 = DIRECTION ( 'NONE',  ( 0.000000000000000000, 0.000000000000000000, -1.000000000000000000 ) ) ;
#13718 = ORIENTED_EDGE ( 'NONE', *, *, #11039, .T. ) ;
#13719 =( REPRESENTATION_RELATIONSHIP ('NONE','NONE', #11251, #13104 ) REPRESENTATION_RELATIONSHIP_WITH_TRANSFORMATION ( #9499 )SHAPE_REPRESENTATION_RELATIONSHIP( ) );
#13720 = CARTESIAN_POINT ( 'NONE',  ( 2.500000000000000000, -1.768423874527825568, -1.020999999999998575 ) ) ;
#13721 = AXIS2_PLACEMENT_3D ( 'NONE', #8814, #11071, #9833 ) ;
#13722 = ORIENTED_EDGE ( 'NONE', *, *, #234, .F. ) ;
#13723 = LINE ( 'NONE', #4818, #1152 ) ;
#13724 = EDGE_CURVE ( 'NONE', #5289, #6984, #6295, .T. ) ;
#13725 = DIRECTION ( 'NONE',  ( -1.000000000000000000, 0.000000000000000000, 0.000000000000000000 ) ) ;
#13726 = COLOUR_RGB ( '',1.000000000000000000, 0.9490196078431372140, 0.9098039215686274384 ) ;
#13727 = ORIENTED_EDGE ( 'NONE', *, *, #9735, .T. ) ;
#13728 = LINE ( 'NONE', #12425, #6420 ) ;
#13729 = ORIENTED_EDGE ( 'NONE', *, *, #14217, .T. ) ;
#13730 = CARTESIAN_POINT ( 'NONE',  ( -314.9999999999999432, 55.00000000000001421, 40.00000000000000000 ) ) ;
#13731 = SURFACE_STYLE_FILL_AREA ( #1607 ) ;
#13732 = LINE ( 'NONE', #2789, #7787 ) ;
#13733 = CIRCLE ( 'NONE', #1922, 13.50000000000000178 ) ;
#13734 = DIRECTION ( 'NONE',  ( -1.000000000000000000, -0.000000000000000000, -0.000000000000000000 ) ) ;
#13735 = DIRECTION ( 'NONE',  ( -1.000000000000000000, 0.000000000000000000, 0.000000000000000000 ) ) ;
#13736 = DIRECTION ( 'NONE',  ( 0.000000000000000000, 0.000000000000000000, -1.000000000000000000 ) ) ;
#13737 = VERTEX_POINT ( 'NONE', #9964 ) ;
#13738 = ORIENTED_EDGE ( 'NONE', *, *, #3116, .F. ) ;
#13739 = EDGE_CURVE ( 'NONE', #11433, #12063, #4451, .T. ) ;
#13740 = SURFACE_SIDE_STYLE ('',( #1620 ) ) ;
#13741 = EDGE_CURVE ( 'NONE', #9112, #5710, #5285, .T. ) ;
#13742 = ORIENTED_EDGE ( 'NONE', *, *, #11065, .T. ) ;
#13743 = FACE_OUTER_BOUND ( 'NONE', #2111, .T. ) ;
#13744 = CARTESIAN_POINT ( 'NONE',  ( -304.9999999999999432, -95.00000000000008527, 354.1421356237308942 ) ) ;
#13745 = FILL_AREA_STYLE ('',( #10414 ) ) ;
#13746 = EDGE_LOOP ( 'NONE', ( #8494, #6837 ) ) ;
#13747 = CARTESIAN_POINT ( 'NONE',  ( -6.259644161404860030E-16, -4.618802153517027165, -5.000000000000000000 ) ) ;
#13748 = ADVANCED_FACE ( 'NONE', ( #14304 ), #6554, .F. ) ;
#13749 = DIRECTION ( 'NONE',  ( -0.000000000000000000, 1.000000000000000000, 0.000000000000000000 ) ) ;
#13750 = DIRECTION ( 'NONE',  ( 1.000000000000000000, 0.000000000000000000, 0.000000000000000000 ) ) ;
#13751 = PLANE ( 'NONE',  #8005 ) ;
#13752 = ORIENTED_EDGE ( 'NONE', *, *, #530, .F. ) ;
#13753 = EDGE_CURVE ( 'NONE', #7324, #5335, #13423, .T. ) ;
#13754 = DIRECTION ( 'NONE',  ( 0.000000000000000000, 0.000000000000000000, 1.000000000000000000 ) ) ;
#13755 = PRODUCT_DEFINITION_SHAPE ( 'NONE', 'NONE',  #14375 ) ;
#13756 = ORIENTED_EDGE ( 'NONE', *, *, #11318, .F. ) ;
#13757 = PLANE ( 'NONE',  #9180 ) ;
#13758 = PRESENTATION_STYLE_ASSIGNMENT (( #14050 ) ) ;
#13759 = PRESENTATION_STYLE_ASSIGNMENT (( #13272 ) ) ;
#13760 = ADVANCED_FACE ( 'NONE', ( #10094 ), #3297, .F. ) ;
#13761 = FACE_OUTER_BOUND ( 'NONE', #3880, .T. ) ;
#13762 = CARTESIAN_POINT ( 'NONE',  ( -3.355112389629170799, 2.681727112203152963, -0.2256878752776689534 ) ) ;
#13763 = CARTESIAN_POINT ( 'NONE',  ( -30.00000000000002842, -25.00000000000000000, 250.0000000000000000 ) ) ;
#13764 = CLOSED_SHELL ( 'NONE', ( #2685, #4027, #2033, #5439, #13455, #3145, #1042, #5216, #4674, #5690, #7849, #9976, #2416, #4106, #416, #8469, #11921, #7053, #13315, #10205, #9598, #2483, #13093, #14275, #11115, #5879, #3328, #4258, #7712, #1237, #13847, #2066 ) ) ;
#13765 = EDGE_CURVE ( 'NONE', #5358, #1004, #2482, .T. ) ;
#13766 = DIRECTION ( 'NONE',  ( -1.000000000000000000, -0.000000000000000000, -0.000000000000000000 ) ) ;
#13767 = ITEM_DEFINED_TRANSFORMATION ( 'NONE', 'NONE', #9794,  #14039 ) ;
#13768 = EDGE_LOOP ( 'NONE', ( #5699, #3083, #13434, #13686 ) ) ;
#13769 = ADVANCED_FACE ( 'NONE', ( #3370 ), #4590, .F. ) ;
#13770 = DIRECTION ( 'NONE',  ( 1.000000000000000000, 0.000000000000000000, -0.000000000000000000 ) ) ;
#13771 = ORIENTED_EDGE ( 'NONE', *, *, #8605, .T. ) ;
#13772 = PLANE ( 'NONE',  #10501 ) ;
#13773 = CARTESIAN_POINT ( 'NONE',  ( 145.5000000000000284, -75.00000000000008527, 190.0000000000000000 ) ) ;
#13774 = APPLICATION_CONTEXT ( 'automotive_design' ) ;
#13775 = ORIENTED_EDGE ( 'NONE', *, *, #9838, .F. ) ;
#13776 = CARTESIAN_POINT ( 'NONE',  ( -1.393927851585477606, 4.043713361053528743, -3.526374918436835149 ) ) ;
#13777 = ORIENTED_EDGE ( 'NONE', *, *, #12271, .T. ) ;
#13778 = DIRECTION ( 'NONE',  ( -0.000000000000000000, -0.000000000000000000, -1.000000000000000000 ) ) ;
#13779 = LINE ( 'NONE', #4949, #7345 ) ;
#13780 = ORIENTED_EDGE ( 'NONE', *, *, #5091, .T. ) ;
#13781 = PRODUCT_DEFINITION_CONTEXT ( 'detailed design', #1632, 'design' ) ;
#13782 = CARTESIAN_POINT ( 'NONE',  ( 211.3397459621556038, -90.00000000000007105, 170.0000000000000000 ) ) ;
#13783 = CARTESIAN_POINT ( 'NONE',  ( 0.000000000000000000, 0.000000000000000000, -25.03750572909317285 ) ) ;
#13784 = SHAPE_REPRESENTATION_RELATIONSHIP ( 'NONE' , 'NONE' ,  #13104, #1425 ) ;
#13785 = CARTESIAN_POINT ( 'NONE',  ( 1.999999999999994893, 0.000000000000000000, -10.72499999999999964 ) ) ;
#13786 = APPLICATION_PROTOCOL_DEFINITION ( 'draft international standard', 'automotive_design', 1998, #12304 ) ;
#13787 = DIRECTION ( 'NONE',  ( 0.000000000000000000, 0.000000000000000000, -1.000000000000000000 ) ) ;
#13788 = ORIENTED_EDGE ( 'NONE', *, *, #1897, .F. ) ;
#13789 = ORIENTED_EDGE ( 'NONE', *, *, #308, .T. ) ;
#13790 = EDGE_LOOP ( 'NONE', ( #3885, #456, #12463, #9486 ) ) ;
#13791 = FACE_BOUND ( 'NONE', #2310, .T. ) ;
#13792 = ADVANCED_FACE ( 'NONE', ( #3230 ), #11256, .T. ) ;
#13793 = ORIENTED_EDGE ( 'NONE', *, *, #7468, .F. ) ;
#13794 = FACE_OUTER_BOUND ( 'NONE', #13705, .T. ) ;
#13795 = VERTEX_POINT ( 'NONE', #7767 ) ;
#13796 = CARTESIAN_POINT ( 'NONE',  ( 2.500000000000000000, 2.357898499370431722, -2.818925648462311528E-15 ) ) ;
#13797 = CONICAL_SURFACE ( 'NONE', #1504, 4.000000000000000000, 0.8911886515913786111 ) ;
#13798 = DIRECTION ( 'NONE',  ( 0.000000000000000000, -3.612465276695121047E-15, 1.000000000000000000 ) ) ;
#13799 = CARTESIAN_POINT ( 'NONE',  ( 1.411581201560190495E-15, 4.862606272033091592, -3.745885042887436622 ) ) ;
#13800 = DIRECTION ( 'NONE',  ( 1.000000000000000000, 0.000000000000000000, 0.000000000000000000 ) ) ;
#13801 = DIRECTION ( 'NONE',  ( 0.000000000000000000, 1.000000000000000000, -1.224646799147353207E-16 ) ) ;
#13802 = CARTESIAN_POINT ( 'NONE',  ( 2.740000000000000213, 0.9838866223910001096, -0.5150000000000001243 ) ) ;
#13803 = AXIS2_PLACEMENT_3D ( 'NONE', #13203, #1141, #186 ) ;
#13804 = ORIENTED_EDGE ( 'NONE', *, *, #10475, .T. ) ;
#13805 = ORIENTED_EDGE ( 'NONE', *, *, #8070, .F. ) ;
#13806 = AXIS2_PLACEMENT_3D ( 'NONE', #10146, #2312, #6553 ) ;
#13807 = VECTOR ( 'NONE', #10922, 1000.000000000000000 ) ;
#13808 = DIRECTION ( 'NONE',  ( 0.000000000000000000, -0.000000000000000000, 1.000000000000000000 ) ) ;
#13809 = CARTESIAN_POINT ( 'NONE',  ( 0.000000000000000000, 0.000000000000000000, -4.000000000000000000 ) ) ;
#13810 = VECTOR ( 'NONE', #3488, 1000.000000000000000 ) ;
#13811 = ORIENTED_EDGE ( 'NONE', *, *, #5803, .T. ) ;
#13812 = DIRECTION ( 'NONE',  ( -0.8949343913984706411, -1.557891129246106096E-15, 0.4461977533473793223 ) ) ;
#13813 = EDGE_CURVE ( 'NONE', #7250, #6282, #3642, .T. ) ;
#13814 = VECTOR ( 'NONE', #8723, 1000.000000000000000 ) ;
#13815 = DIRECTION ( 'NONE',  ( 1.000000000000000000, 0.000000000000000000, 0.000000000000000000 ) ) ;
#13816 = DIRECTION ( 'NONE',  ( 6.123233995736766036E-17, 0.000000000000000000, 1.000000000000000000 ) ) ;
#13817 = EDGE_CURVE ( 'NONE', #6984, #2940, #2501, .T. ) ;
#13818 = CARTESIAN_POINT ( 'NONE',  ( 181.0000000000000000, -8.660254037844389075, 199.9990000000000236 ) ) ;
#13819 = CARTESIAN_POINT ( 'NONE',  ( 347.0000000000000000, 8.660254037844390851, 199.9990000000000236 ) ) ;
#13820 = VECTOR ( 'NONE', #8288, 1000.000000000000000 ) ;
#13821 = ORIENTED_EDGE ( 'NONE', *, *, #3986, .T. ) ;
#13822 = CARTESIAN_POINT ( 'NONE',  ( 0.000000000000000000, -2.349999999999999201, -0.5150000000000000133 ) ) ;
#13823 = AXIS2_PLACEMENT_3D ( 'NONE', #12278, #6972, #9147 ) ;
#13824 = DIRECTION ( 'NONE',  ( -1.000000000000000000, 0.000000000000000000, -0.000000000000000000 ) ) ;
#13825 = AXIS2_PLACEMENT_3D ( 'NONE', #6133, #1549, #11501 ) ;
#13826 = AXIS2_PLACEMENT_3D ( 'NONE', #4383, #7631, #1233 ) ;
#13827 = ORIENTED_EDGE ( 'NONE', *, *, #685, .T. ) ;
#13828 = FACE_OUTER_BOUND ( 'NONE', #11167, .T. ) ;
#13829 = FILL_AREA_STYLE ('',( #10655 ) ) ;
#13830 = AXIS2_PLACEMENT_3D ( 'NONE', #3236, #6487, #874 ) ;
#13831 = FACE_OUTER_BOUND ( 'NONE', #7867, .T. ) ;
#13832 = EDGE_CURVE ( 'NONE', #9294, #9773, #4520, .T. ) ;
#13833 = DIRECTION ( 'NONE',  ( 0.000000000000000000, 0.000000000000000000, 1.000000000000000000 ) ) ;
#13834 = EDGE_CURVE ( 'NONE', #13189, #145, #3846, .T. ) ;
#13835 = VECTOR ( 'NONE', #5020, 1000.000000000000000 ) ;
#13836 = DIRECTION ( 'NONE',  ( 0.000000000000000000, 0.000000000000000000, 1.000000000000000000 ) ) ;
#13837 = PLANE ( 'NONE',  #5085 ) ;
#13838 = CARTESIAN_POINT ( 'NONE',  ( 4.000000000000000000, 0.9868501483902631932, -0.09357334158579604100 ) ) ;
#13839 = CONTEXT_DEPENDENT_SHAPE_REPRESENTATION ( #6783, #6488 ) ;
#13840 = EDGE_CURVE ( 'NONE', #247, #6636, #6433, .T. ) ;
#13841 = ORIENTED_EDGE ( 'NONE', *, *, #12601, .F. ) ;
#13842 = PLANE ( 'NONE',  #12629 ) ;
#13843 = VERTEX_POINT ( 'NONE', #2627 ) ;
#13844 = DIRECTION ( 'NONE',  ( -1.000000000000000000, 0.000000000000000000, 0.000000000000000000 ) ) ;
#13845 = CARTESIAN_POINT ( 'NONE',  ( 2.500000000000000000, 1.178949249685213863, -2.042000000000001148 ) ) ;
#13846 = EDGE_CURVE ( 'NONE', #3377, #12061, #10303, .T. ) ;
#13847 = ADVANCED_FACE ( 'NONE', ( #271 ), #9447, .F. ) ;
#13848 = EDGE_LOOP ( 'NONE', ( #8542, #4371, #4116, #53 ) ) ;
#13849 = EDGE_CURVE ( 'NONE', #6716, #11552, #2018, .T. ) ;
#13850 = LINE ( 'NONE', #6310, #5972 ) ;
#13851 = ORIENTED_EDGE ( 'NONE', *, *, #14017, .T. ) ;
#13852 = ADVANCED_FACE ( 'NONE', ( #2551 ), #7180, .F. ) ;
#13853 = FACE_OUTER_BOUND ( 'NONE', #2144, .T. ) ;
#13854 = CARTESIAN_POINT ( 'NONE',  ( -4.000000000000000000, 2.309401076758498483, -0.4999999999999927280 ) ) ;
#13855 = EDGE_LOOP ( 'NONE', ( #2679, #7527, #4459, #2401 ) ) ;
#13856 = LINE ( 'NONE', #3712, #4119 ) ;
#13857 = DIRECTION ( 'NONE',  ( 1.000000000000000000, 0.000000000000000000, 0.000000000000000000 ) ) ;
#13858 = PRESENTATION_STYLE_ASSIGNMENT (( #7261 ) ) ;
#13859 = APPLICATION_PROTOCOL_DEFINITION ( 'draft international standard', 'automotive_design', 1998, #12764 ) ;
#13860 = CARTESIAN_POINT ( 'NONE',  ( 1.567478505476134606E-15, 4.618802153517012066, -3.433295621305382905 ) ) ;
#13861 = ORIENTED_EDGE ( 'NONE', *, *, #11387, .T. ) ;
#13862 = ORIENTED_EDGE ( 'NONE', *, *, #6755, .T. ) ;
#13863 = AXIS2_PLACEMENT_3D ( 'NONE', #2128, #13355, #12072 ) ;
#13864 = LINE ( 'NONE', #12849, #6601 ) ;
#13865 = ORIENTED_EDGE ( 'NONE', *, *, #11621, .F. ) ;
#13866 = DIRECTION ( 'NONE',  ( 0.000000000000000000, 0.000000000000000000, 1.000000000000000000 ) ) ;
#13867 = AXIS2_PLACEMENT_3D ( 'NONE', #8927, #4574, #4710 ) ;
#13868 = ORIENTED_EDGE ( 'NONE', *, *, #4975, .F. ) ;
#13869 = DIRECTION ( 'NONE',  ( -1.000000000000000000, 0.000000000000000000, 0.000000000000000000 ) ) ;
#13870 = ORIENTED_EDGE ( 'NONE', *, *, #12512, .T. ) ;
#13871 = DIRECTION ( 'NONE',  ( -1.000000000000000000, 0.000000000000000000, 0.000000000000000000 ) ) ;
#13872 = DIRECTION ( 'NONE',  ( -0.000000000000000000, -0.000000000000000000, -1.000000000000000000 ) ) ;
#13873 = DIRECTION ( 'NONE',  ( -0.000000000000000000, -0.000000000000000000, -1.000000000000000000 ) ) ;
#13874 = LINE ( 'NONE', #3950, #1648 ) ;
#13875 = CARTESIAN_POINT ( 'NONE',  ( 0.000000000000000000, 0.000000000000000000, 190.0000000000000000 ) ) ;
#13876 = AXIS2_PLACEMENT_3D ( 'NONE', #9789, #7737, #8688 ) ;
#13877 = FACE_OUTER_BOUND ( 'NONE', #8648, .T. ) ;
#13878 = PRODUCT_DEFINITION_SHAPE ( 'NONE', 'NONE',  #14367 ) ;
#13879 = ORIENTED_EDGE ( 'NONE', *, *, #717, .T. ) ;
#13880 = ADVANCED_FACE ( 'NONE', ( #332 ), #11542, .F. ) ;
#13881 = VERTEX_POINT ( 'NONE', #2693 ) ;
#13882 = FACE_OUTER_BOUND ( 'NONE', #14168, .T. ) ;
#13883 = DIRECTION ( 'NONE',  ( 0.000000000000000000, 0.000000000000000000, -1.000000000000000000 ) ) ;
#13884 = CIRCLE ( 'NONE', #8569, 4.750000000000000000 ) ;
#13885 = DIRECTION ( 'NONE',  ( -0.000000000000000000, 1.000000000000000000, -0.000000000000000000 ) ) ;
#13886 = FACE_OUTER_BOUND ( 'NONE', #12360, .T. ) ;
#13887 = ORIENTED_EDGE ( 'NONE', *, *, #1415, .F. ) ;
#13888 = CIRCLE ( 'NONE', #10416, 2.649999999999985700 ) ;
#13889 = AXIS2_PLACEMENT_3D ( 'NONE', #12282, #131, #3441 ) ;
#13890 = DIRECTION ( 'NONE',  ( 1.000000000000000000, 0.000000000000000000, -0.000000000000000000 ) ) ;
#13891 = LINE ( 'NONE', #6211, #9956 ) ;
#13892 = DIRECTION ( 'NONE',  ( 6.123233995736766036E-17, -1.000000000000000000, 0.000000000000000000 ) ) ;
#13893 = DIRECTION ( 'NONE',  ( 0.000000000000000000, 0.000000000000000000, -1.000000000000000000 ) ) ;
#13894 = CARTESIAN_POINT ( 'NONE',  ( 357.0000000000000000, 8.660254037844390851, 199.9990000000000236 ) ) ;
#13895 = VERTEX_POINT ( 'NONE', #5884 ) ;
#13896 = CARTESIAN_POINT ( 'NONE',  ( 233.8499999999999375, -85.00000000000007105, 55.00000000000001421 ) ) ;
#13897 = AXIS2_PLACEMENT_3D ( 'NONE', #2748, #688, #12896 ) ;
#13898 = DIRECTION ( 'NONE',  ( 0.000000000000000000, 0.000000000000000000, 1.000000000000000000 ) ) ;
#13899 = EDGE_CURVE ( 'NONE', #11802, #9015, #13132, .T. ) ;
#13900 = EDGE_LOOP ( 'NONE', ( #14131, #1389 ) ) ;
#13901 = DIRECTION ( 'NONE',  ( 0.000000000000000000, 0.000000000000000000, 1.000000000000000000 ) ) ;
#13902 = DIRECTION ( 'NONE',  ( 1.000000000000000000, 0.000000000000000000, 0.000000000000000000 ) ) ;
#13903 = CONICAL_SURFACE ( 'NONE', #3272, 3077.683537175319998, 1.256637061435923686 ) ;
#13904 =( REPRESENTATION_RELATIONSHIP ('NONE','NONE', #11251, #10796 ) REPRESENTATION_RELATIONSHIP_WITH_TRANSFORMATION ( #2013 )SHAPE_REPRESENTATION_RELATIONSHIP( ) );
#13905 = DIRECTION ( 'NONE',  ( 0.000000000000000000, 1.000000000000000000, 0.000000000000000000 ) ) ;
#13906 = CARTESIAN_POINT ( 'NONE',  ( 319.9999999999999432, -24.99999999999999289, 19.99999999999998934 ) ) ;
#13907 = DIRECTION ( 'NONE',  ( -0.8191520442889875797, 1.003171929053519570E-16, 0.5735764363510522656 ) ) ;
#13908 = CARTESIAN_POINT ( 'NONE',  ( -140.0000000000000000, -75.00000000000008527, 30.00000000000000000 ) ) ;
#13909 = PRESENTATION_LAYER_ASSIGNMENT (  '', '', ( #10207 ) ) ;
#13910 = DIRECTION ( 'NONE',  ( 1.000000000000000000, 0.000000000000000000, 0.000000000000000000 ) ) ;
#13911 = ORIENTED_EDGE ( 'NONE', *, *, #7170, .F. ) ;
#13912 = FACE_OUTER_BOUND ( 'NONE', #8066, .T. ) ;
#13913 = AXIS2_PLACEMENT_3D ( 'NONE', #12306, #13451, #4543 ) ;
#13914 = ORIENTED_EDGE ( 'NONE', *, *, #4202, .F. ) ;
#13915 = DIRECTION ( 'NONE',  ( -0.000000000000000000, -0.000000000000000000, -1.000000000000000000 ) ) ;
#13916 = DIRECTION ( 'NONE',  ( -1.000000000000000000, 0.000000000000000000, 0.000000000000000000 ) ) ;
#13917 = ADVANCED_FACE ( 'NONE', ( #9221 ), #7043, .F. ) ;
#13918 = ORIENTED_EDGE ( 'NONE', *, *, #1162, .F. ) ;
#13919 = DIRECTION ( 'NONE',  ( 0.000000000000000000, 0.000000000000000000, 1.000000000000000000 ) ) ;
#13920 = ORIENTED_EDGE ( 'NONE', *, *, #339, .T. ) ;
#13921 = MECHANICAL_DESIGN_GEOMETRIC_PRESENTATION_REPRESENTATION (  '', ( #12541 ), #4413 ) ;
#13922 = CARTESIAN_POINT ( 'NONE',  ( 299.9999999999999432, -95.00000000000008527, 186.2999999999999829 ) ) ;
#13923 = DIRECTION ( 'NONE',  ( 0.000000000000000000, -0.4999999999999993339, 0.8660254037844390407 ) ) ;
#13924 = VERTEX_POINT ( 'NONE', #8268 ) ;
#13925 = CARTESIAN_POINT ( 'NONE',  ( 10.00000000000000000, 1.224646799147353256E-15, -200.0000000000000000 ) ) ;
#13926 = DIRECTION ( 'NONE',  ( 0.000000000000000000, 0.000000000000000000, -1.000000000000000000 ) ) ;
#13927 = VECTOR ( 'NONE', #3248, 1000.000000000000000 ) ;
#13928 = SURFACE_SIDE_STYLE ('',( #781 ) ) ;
#13929 = APPLICATION_PROTOCOL_DEFINITION ( 'draft international standard', 'automotive_design', 1998, #1924 ) ;
#13930 = EDGE_CURVE ( 'NONE', #1900, #7098, #13779, .T. ) ;
#13931 = EDGE_CURVE ( 'NONE', #10087, #12612, #12213, .T. ) ;
#13932 = DIRECTION ( 'NONE',  ( -1.000000000000000000, -0.000000000000000000, -0.000000000000000000 ) ) ;
#13933 = ORIENTED_EDGE ( 'NONE', *, *, #8333, .F. ) ;
#13934 = AXIS2_PLACEMENT_3D ( 'NONE', #5956, #3849, #8271 ) ;
#13935 = EDGE_CURVE ( 'NONE', #12519, #11189, #9368, .T. ) ;
#13936 = ORIENTED_EDGE ( 'NONE', *, *, #2410, .F. ) ;
#13937 = VERTEX_POINT ( 'NONE', #4877 ) ;
#13938 = EDGE_LOOP ( 'NONE', ( #8886, #1734 ) ) ;
#13939 = LINE ( 'NONE', #9671, #7649 ) ;
#13940 = CIRCLE ( 'NONE', #13017, 2.500000000000002220 ) ;
#13941 = ORIENTED_EDGE ( 'NONE', *, *, #4992, .T. ) ;
#13942 = CARTESIAN_POINT ( 'NONE',  ( 0.000000000000000000, 0.000000000000000000, -190.0000000000000000 ) ) ;
#13943 = VERTEX_POINT ( 'NONE', #6970 ) ;
#13944 = DIRECTION ( 'NONE',  ( -0.000000000000000000, -0.000000000000000000, 1.000000000000000000 ) ) ;
#13945 = AXIS2_PLACEMENT_3D ( 'NONE', #8689, #6728, #4491 ) ;
#13946 = CARTESIAN_POINT ( 'NONE',  ( -4.000000000000000000, 2.309401076758498483, -5.000000000000000000 ) ) ;
#13947 = CARTESIAN_POINT ( 'NONE',  ( 3.510273485745307731, 2.827716139362654424, -3.610536846335885564 ) ) ;
#13948 = CYLINDRICAL_SURFACE ( 'NONE', #1418, 2.649999999999985700 ) ;
#13949 = CARTESIAN_POINT ( 'NONE',  ( 219.9999999999999147, -85.00000000000009948, -18.00000000000000355 ) ) ;
#13950 = EDGE_CURVE ( 'NONE', #1808, #9732, #4339, .T. ) ;
#13951 = CARTESIAN_POINT ( 'NONE',  ( 53.33333333333330017, -20.00000000000000000, -219.8500000000001080 ) ) ;
#13952 = AXIS2_PLACEMENT_3D ( 'NONE', #10491, #2877, #4980 ) ;
#13953 = EDGE_CURVE ( 'NONE', #7861, #6913, #601, .T. ) ;
#13954 = ORIENTED_EDGE ( 'NONE', *, *, #4907, .F. ) ;
#13955 = ORIENTED_EDGE ( 'NONE', *, *, #3623, .F. ) ;
#13956 = LINE ( 'NONE', #2272, #4937 ) ;
#13957 = COLOUR_RGB ( '',1.000000000000000000, 0.9490196078431372140, 0.9098039215686274384 ) ;
#13958 = CIRCLE ( 'NONE', #5402, 2.649999999999985700 ) ;
#13959 = EDGE_CURVE ( 'NONE', #5006, #9071, #12441, .T. ) ;
#13960 = CARTESIAN_POINT ( 'NONE',  ( 2.500000000000000000, -1.178949249685213863, 2.042000000000002924 ) ) ;
#13961 = EDGE_LOOP ( 'NONE', ( #282, #9864 ) ) ;
#13962 = DIRECTION ( 'NONE',  ( -0.000000000000000000, -0.000000000000000000, 1.000000000000000000 ) ) ;
#13963 = DIRECTION ( 'NONE',  ( 0.000000000000000000, 0.000000000000000000, -1.000000000000000000 ) ) ;
#13964 = AXIS2_PLACEMENT_3D ( 'NONE', #6271, #5054, #14167 ) ;
#13965 = DIRECTION ( 'NONE',  ( 1.000000000000000000, 0.000000000000000000, 0.000000000000000000 ) ) ;
#13966 = ORIENTED_EDGE ( 'NONE', *, *, #13959, .T. ) ;
#13967 = SURFACE_STYLE_USAGE ( .BOTH. , #11058 ) ;
#13968 = FACE_OUTER_BOUND ( 'NONE', #1898, .T. ) ;
#13969 = DIRECTION ( 'NONE',  ( -0.000000000000000000, 0.000000000000000000, 1.000000000000000000 ) ) ;
#13970 = CARTESIAN_POINT ( 'NONE',  ( 0.000000000000000000, 0.000000000000000000, 139.9999999999999716 ) ) ;
#13971 = CARTESIAN_POINT ( 'NONE',  ( 0.000000000000000000, 0.000000000000000000, -186.0000000000000000 ) ) ;
#13972 = VERTEX_POINT ( 'NONE', #5740 ) ;
#13973 = ORIENTED_EDGE ( 'NONE', *, *, #2005, .T. ) ;
#13974 = DIRECTION ( 'NONE',  ( 0.000000000000000000, -1.287488025362403787E-15, -1.000000000000000000 ) ) ;
#13975 = EDGE_CURVE ( 'NONE', #6255, #10103, #8192, .T. ) ;
#13976 = ORIENTED_EDGE ( 'NONE', *, *, #9965, .T. ) ;
#13977 = DIRECTION ( 'NONE',  ( -0.000000000000000000, -0.000000000000000000, -1.000000000000000000 ) ) ;
#13978 = DIRECTION ( 'NONE',  ( 0.000000000000000000, 0.000000000000000000, -1.000000000000000000 ) ) ;
#13979 = CARTESIAN_POINT ( 'NONE',  ( -3.861362476283256129, -2.629030857716004199, -3.671615880910374941 ) ) ;
#13980 = DIRECTION ( 'NONE',  ( 0.000000000000000000, 0.000000000000000000, 1.000000000000000000 ) ) ;
#13981 = CARTESIAN_POINT ( 'NONE',  ( -2.725741868435985094, 3.045094352034055429, -3.220599429844047012 ) ) ;
#13982 = CONTEXT_DEPENDENT_SHAPE_REPRESENTATION ( #10204, #9845 ) ;
#13983 = VERTEX_POINT ( 'NONE', #201 ) ;
#13984 = FACE_BOUND ( 'NONE', #5111, .T. ) ;
#13985 = ORIENTED_EDGE ( 'NONE', *, *, #13054, .T. ) ;
#13986 = DIRECTION ( 'NONE',  ( 1.000000000000000000, 0.000000000000000000, 0.000000000000000000 ) ) ;
#13987 = LINE ( 'NONE', #12616, #1668 ) ;
#13988 = ORIENTED_EDGE ( 'NONE', *, *, #7667, .T. ) ;
#13989 = DIRECTION ( 'NONE',  ( -1.000000000000000000, -0.000000000000000000, -0.000000000000000000 ) ) ;
#13990 = ORIENTED_EDGE ( 'NONE', *, *, #972, .F. ) ;
#13991 = DIRECTION ( 'NONE',  ( -0.000000000000000000, -0.000000000000000000, -1.000000000000000000 ) ) ;
#13992 = PRODUCT_DEFINITION_SHAPE ( 'NONE', 'NONE',  #14361 ) ;
#13993 = DIRECTION ( 'NONE',  ( 0.000000000000000000, 0.000000000000000000, 1.000000000000000000 ) ) ;
#13994 = EDGE_LOOP ( 'NONE', ( #12949, #8264 ) ) ;
#13995 = DIRECTION ( 'NONE',  ( 0.000000000000000000, 0.000000000000000000, -1.000000000000000000 ) ) ;
#13996 =( NAMED_UNIT ( * ) SI_UNIT ( $, .STERADIAN. ) SOLID_ANGLE_UNIT ( ) );
#13997 = EDGE_CURVE ( 'NONE', #682, #11608, #9076, .T. ) ;
#13998 = CARTESIAN_POINT ( 'NONE',  ( 10.00000000000000000, 1.224646799147353256E-15, 200.0000000000000000 ) ) ;
#13999 = EDGE_CURVE ( 'NONE', #4356, #11323, #1268, .T. ) ;
#14000 = ORIENTED_EDGE ( 'NONE', *, *, #5925, .F. ) ;
#14001 = ORIENTED_EDGE ( 'NONE', *, *, #14011, .F. ) ;
#14002 = CARTESIAN_POINT ( 'NONE',  ( 0.000000000000000000, 0.000000000000000000, 11.75000000000000000 ) ) ;
#14003 = CIRCLE ( 'NONE', #7967, 2.500000000000000000 ) ;
#14004 = ORIENTED_EDGE ( 'NONE', *, *, #3806, .T. ) ;
#14005 = FACE_BOUND ( 'NONE', #9951, .T. ) ;
#14006 = ORIENTED_EDGE ( 'NONE', *, *, #8167, .F. ) ;
#14007 = VERTEX_POINT ( 'NONE', #14070 ) ;
#14008 = LINE ( 'NONE', #5039, #11748 ) ;
#14009 = EDGE_LOOP ( 'NONE', ( #10254, #9706 ) ) ;
#14010 = DIRECTION ( 'NONE',  ( 1.000000000000000000, 0.000000000000000000, 0.000000000000000000 ) ) ;
#14011 = EDGE_CURVE ( 'NONE', #5369, #12491, #11750, .T. ) ;
#14012 = CARTESIAN_POINT ( 'NONE',  ( -30.00000000000002842, -225.0000000000000000, -169.9999999999999716 ) ) ;
#14013 = DIRECTION ( 'NONE',  ( -0.000000000000000000, 0.000000000000000000, 1.000000000000000000 ) ) ;
#14014 = AXIS2_PLACEMENT_3D ( 'NONE', #8403, #12613, #3775 ) ;
#14015 = FACE_OUTER_BOUND ( 'NONE', #10138, .T. ) ;
#14016 = EDGE_CURVE ( 'NONE', #4963, #7321, #3401, .T. ) ;
#14017 = EDGE_CURVE ( 'NONE', #6282, #7250, #4123, .T. ) ;
#14018 = CARTESIAN_POINT ( 'NONE',  ( 142.6500000000000057, -95.00000000000008527, 186.2999999999999829 ) ) ;
#14019 = ORIENTED_EDGE ( 'NONE', *, *, #326, .F. ) ;
#14020 = ORIENTED_EDGE ( 'NONE', *, *, #13228, .F. ) ;
#14021 = CYLINDRICAL_SURFACE ( 'NONE', #12811, 9.999999999999996447 ) ;
#14022 = AXIS2_PLACEMENT_3D ( 'NONE', #10984, #1975, #7494 ) ;
#14023 = AXIS2_PLACEMENT_3D ( 'NONE', #8015, #10209, #5784 ) ;
#14024 = ORIENTED_EDGE ( 'NONE', *, *, #9861, .T. ) ;
#14025 = DIRECTION ( 'NONE',  ( -1.000000000000000000, -0.000000000000000000, -0.000000000000000000 ) ) ;
#14026 = CARTESIAN_POINT ( 'NONE',  ( -134.9999999999999716, 45.00000000000001421, 30.00000000000000000 ) ) ;
#14027 = EDGE_CURVE ( 'NONE', #14086, #6723, #10959, .T. ) ;
#14028 = ADVANCED_FACE ( 'NONE', ( #1660 ), #6101, .T. ) ;
#14029 = LINE ( 'NONE', #9767, #12232 ) ;
#14030 = ORIENTED_EDGE ( 'NONE', *, *, #1331, .T. ) ;
#14031 = EDGE_CURVE ( 'NONE', #4659, #11887, #5017, .T. ) ;
#14032 = EDGE_CURVE ( 'NONE', #1298, #1984, #7356, .T. ) ;
#14033 = FACE_OUTER_BOUND ( 'NONE', #13360, .T. ) ;
#14034 = EDGE_CURVE ( 'NONE', #12590, #5504, #8339, .T. ) ;
#14035 = VECTOR ( 'NONE', #13778, 1000.000000000000000 ) ;
#14036 = DIRECTION ( 'NONE',  ( -1.000000000000000000, 0.000000000000000000, 0.000000000000000000 ) ) ;
#14037 = DIRECTION ( 'NONE',  ( -1.000000000000000000, 0.000000000000000000, 6.123233995736766036E-17 ) ) ;
#14038 = DIRECTION ( 'NONE',  ( -1.000000000000000000, 0.000000000000000000, 0.000000000000000000 ) ) ;
#14039 = AXIS2_PLACEMENT_3D ( 'NONE', #10508, #9418, #5077 ) ;
#14040 = ORIENTED_EDGE ( 'NONE', *, *, #4726, .F. ) ;
#14041 = ORIENTED_EDGE ( 'NONE', *, *, #3988, .T. ) ;
#14042 = LINE ( 'NONE', #9844, #14130 ) ;
#14043 = AXIS2_PLACEMENT_3D ( 'NONE', #6748, #2659, #10275 ) ;
#14044 = DIRECTION ( 'NONE',  ( -0.000000000000000000, -1.000000000000000000, -0.000000000000000000 ) ) ;
#14045 = CIRCLE ( 'NONE', #11505, 12.44999999999999929 ) ;
#14046 = PRODUCT_DEFINITION_CONTEXT ( 'detailed design', #5364, 'design' ) ;
#14047 = ORIENTED_EDGE ( 'NONE', *, *, #14294, .T. ) ;
#14048 = DIRECTION ( 'NONE',  ( -0.000000000000000000, -0.000000000000000000, -1.000000000000000000 ) ) ;
#14049 = AXIS2_PLACEMENT_3D ( 'NONE', #10180, #10318, #8206 ) ;
#14050 = SURFACE_STYLE_USAGE ( .BOTH. , #3978 ) ;
#14051 = CARTESIAN_POINT ( 'NONE',  ( 0.6666666666666658525, -4.233901974057276085, -3.300726591567086476 ) ) ;
#14052 = CARTESIAN_POINT ( 'NONE',  ( 219.9999999999999716, -20.00000000000000000, 222.5000000000000853 ) ) ;
#14053 = CARTESIAN_POINT ( 'NONE',  ( 2.500000000000000000, 0.000000000000000000, 2.041999999999999815 ) ) ;
#14054 = AXIS2_PLACEMENT_3D ( 'NONE', #12427, #11210, #6708 ) ;
#14055 = CIRCLE ( 'NONE', #10604, 2.055000000000000160 ) ;
#14056 = ADVANCED_FACE ( 'NONE', ( #2840 ), #6664, .T. ) ;
#14057 = EDGE_LOOP ( 'NONE', ( #2190, #4064, #11229, #4838 ) ) ;
#14058 = CIRCLE ( 'NONE', #4576, 2.500000000000002220 ) ;
#14059 = DIRECTION ( 'NONE',  ( 0.000000000000000000, 0.000000000000000000, 1.000000000000000000 ) ) ;
#14060 = AXIS2_PLACEMENT_3D ( 'NONE', #2341, #2147, #13222 ) ;
#14061 = EDGE_LOOP ( 'NONE', ( #10678, #10464, #12493, #12630 ) ) ;
#14062 = CARTESIAN_POINT ( 'NONE',  ( -299.9999999999999432, -75.00000000000008527, 0.000000000000000000 ) ) ;
#14063 = PLANE ( 'NONE',  #7863 ) ;
#14064 = AXIS2_PLACEMENT_3D ( 'NONE', #13642, #11201, #1522 ) ;
#14065 = VERTEX_POINT ( 'NONE', #6315 ) ;
#14066 = DIRECTION ( 'NONE',  ( -0.000000000000000000, 0.000000000000000000, 1.000000000000000000 ) ) ;
#14067 = ORIENTED_EDGE ( 'NONE', *, *, #9777, .T. ) ;
#14068 = DIRECTION ( 'NONE',  ( 0.000000000000000000, -1.000000000000000000, 0.000000000000000000 ) ) ;
#14069 = AXIS2_PLACEMENT_3D ( 'NONE', #7884, #7750, #3483 ) ;
#14070 = CARTESIAN_POINT ( 'NONE',  ( 303.3333333333333144, -25.00000000000000000, -225.1500000000000625 ) ) ;
#14071 = ORIENTED_EDGE ( 'NONE', *, *, #12154, .F. ) ;
#14072 = DIRECTION ( 'NONE',  ( 1.000000000000000000, 0.000000000000000000, 0.000000000000000000 ) ) ;
#14073 = VECTOR ( 'NONE', #7865, 1000.000000000000000 ) ;
#14074 = CARTESIAN_POINT ( 'NONE',  ( 4.197393957002303999, 0.8151795401431359833, -3.503767560748935139 ) ) ;
#14075 =( NAMED_UNIT ( * ) SI_UNIT ( $, .STERADIAN. ) SOLID_ANGLE_UNIT ( ) );
#14076 = ITEM_DEFINED_TRANSFORMATION ( 'NONE', 'NONE', #3072,  #14039 ) ;
#14077 = DIRECTION ( 'NONE',  ( 1.000000000000000000, 0.000000000000000000, 0.000000000000000000 ) ) ;
#14078 = EDGE_CURVE ( 'NONE', #4429, #12208, #7085, .T. ) ;
#14079 = VERTEX_POINT ( 'NONE', #3062 ) ;
#14080 = EDGE_LOOP ( 'NONE', ( #10141, #8232 ) ) ;
#14081 = DIRECTION ( 'NONE',  ( -1.000000000000000000, 0.000000000000000000, 0.000000000000000000 ) ) ;
#14082 = AXIS2_PLACEMENT_3D ( 'NONE', #540, #13689, #12540 ) ;
#14083 = ORIENTED_EDGE ( 'NONE', *, *, #8251, .T. ) ;
#14084 = DIRECTION ( 'NONE',  ( 0.000000000000000000, -0.000000000000000000, 1.000000000000000000 ) ) ;
#14085 = UNCERTAINTY_MEASURE_WITH_UNIT (LENGTH_MEASURE( 1.000000000000000082E-05 ), #5987, 'distance_accuracy_value', 'NONE');
#14086 = VERTEX_POINT ( 'NONE', #706 ) ;
#14087 = AXIS2_PLACEMENT_3D ( 'NONE', #2423, #7782, #8815 ) ;
#14088 = ORIENTED_EDGE ( 'NONE', *, *, #9227, .F. ) ;
#14089 = CARTESIAN_POINT ( 'NONE',  ( 0.000000000000000000, -1.178949249685213863, 2.042000000000002924 ) ) ;
#14090 = EDGE_LOOP ( 'NONE', ( #420, #5992, #5075, #9667 ) ) ;
#14091 = EDGE_CURVE ( 'NONE', #6979, #161, #1043, .T. ) ;
#14092 = FACE_OUTER_BOUND ( 'NONE', #6253, .T. ) ;
#14093 = LINE ( 'NONE', #12857, #5072 ) ;
#14094 = DIRECTION ( 'NONE',  ( 1.000000000000000000, 0.000000000000000000, 0.000000000000000000 ) ) ;
#14095 = DIRECTION ( 'NONE',  ( -0.000000000000000000, -0.000000000000000000, -1.000000000000000000 ) ) ;
#14096 = CARTESIAN_POINT ( 'NONE',  ( 203.5000000000000000, -85.00000000000007105, 55.00000000000001421 ) ) ;
#14097 = EDGE_LOOP ( 'NONE', ( #8255, #384, #2979, #5639 ) ) ;
#14098 = ORIENTED_EDGE ( 'NONE', *, *, #5467, .T. ) ;
#14099 = DIRECTION ( 'NONE',  ( -0.000000000000000000, 0.000000000000000000, 1.000000000000000000 ) ) ;
#14100 = EDGE_LOOP ( 'NONE', ( #5109, #13160 ) ) ;
#14101 = FACE_OUTER_BOUND ( 'NONE', #12637, .T. ) ;
#14102 = EDGE_CURVE ( 'NONE', #12266, #1400, #11080, .T. ) ;
#14103 = DIRECTION ( 'NONE',  ( 0.000000000000000000, 0.000000000000000000, -1.000000000000000000 ) ) ;
#14104 = ORIENTED_EDGE ( 'NONE', *, *, #9865, .T. ) ;
#14105 = AXIS2_PLACEMENT_3D ( 'NONE', #12545, #11319, #12609 ) ;
#14106 = CARTESIAN_POINT ( 'NONE',  ( 0.000000000000000000, 0.000000000000000000, 30.00000000000000000 ) ) ;
#14107 = CARTESIAN_POINT ( 'NONE',  ( 299.9999999999999432, -95.00000000000008527, 169.9999999999999716 ) ) ;
#14108 = DIRECTION ( 'NONE',  ( 1.000000000000000000, 0.000000000000000000, 6.123233995736766036E-17 ) ) ;
#14109 = DIRECTION ( 'NONE',  ( 0.000000000000000000, 0.000000000000000000, -1.000000000000000000 ) ) ;
#14110 = ADVANCED_FACE ( 'NONE', ( #7323 ), #9587, .F. ) ;
#14111 = EDGE_CURVE ( 'NONE', #6636, #2861, #819, .T. ) ;
#14112 = ORIENTED_EDGE ( 'NONE', *, *, #8251, .F. ) ;
#14113 = EDGE_CURVE ( 'NONE', #840, #1382, #11044, .T. ) ;
#14114 = ORIENTED_EDGE ( 'NONE', *, *, #8317, .F. ) ;
#14115 = VECTOR ( 'NONE', #5496, 1000.000000000000000 ) ;
#14116 = DIRECTION ( 'NONE',  ( 0.000000000000000000, 0.000000000000000000, 1.000000000000000000 ) ) ;
#14117 = DIRECTION ( 'NONE',  ( 1.000000000000000000, 0.000000000000000000, 0.000000000000000000 ) ) ;
#14118 = ORIENTED_EDGE ( 'NONE', *, *, #12321, .T. ) ;
#14119 = CARTESIAN_POINT ( 'NONE',  ( 297.3499999999999659, -95.00000000000008527, -169.9999999999999716 ) ) ;
#14120 = CARTESIAN_POINT ( 'NONE',  ( 386.6666666666666288, -14.99999999999999822, 225.1500000000000625 ) ) ;
#14121 = CIRCLE ( 'NONE', #9032, 1.050000000000000488 ) ;
#14122 = ITEM_DEFINED_TRANSFORMATION ( 'NONE', 'NONE', #2136,  #14039 ) ;
#14123 = AXIS2_PLACEMENT_3D ( 'NONE', #10681, #9448, #712 ) ;
#14124 = ORIENTED_EDGE ( 'NONE', *, *, #11196, .T. ) ;
#14125 = DIRECTION ( 'NONE',  ( -0.000000000000000000, 0.000000000000000000, -1.000000000000000000 ) ) ;
#14126 = ORIENTED_EDGE ( 'NONE', *, *, #3644, .F. ) ;
#14127 = DIRECTION ( 'NONE',  ( 0.000000000000000000, 0.000000000000000000, 1.000000000000000000 ) ) ;
#14128 = DIRECTION ( 'NONE',  ( 0.000000000000000000, -1.000000000000000000, 1.287488025362403787E-15 ) ) ;
#14129 = CIRCLE ( 'NONE', #7185, 2.500000000000002220 ) ;
#14130 = VECTOR ( 'NONE', #8680, 1000.000000000000000 ) ;
#14131 = ORIENTED_EDGE ( 'NONE', *, *, #5577, .T. ) ;
#14132 = DIRECTION ( 'NONE',  ( 0.000000000000000000, -0.4999999999999993894, 0.8660254037844389297 ) ) ;
#14133 = ORIENTED_EDGE ( 'NONE', *, *, #6119, .T. ) ;
#14134 = CARTESIAN_POINT ( 'NONE',  ( 297.3499999999999659, -75.00000000000008527, -169.9999999999999716 ) ) ;
#14135 = CARTESIAN_POINT ( 'NONE',  ( -4.000000000000000000, 0.9868501483902560878, -0.09357334158579519445 ) ) ;
#14136 = EDGE_LOOP ( 'NONE', ( #10388, #11160, #6396, #3796 ) ) ;
#14137 = FACE_BOUND ( 'NONE', #5955, .T. ) ;
#14138 = ADVANCED_FACE ( 'NONE', ( #13402 ), #2176, .T. ) ;
#14139 = AXIS2_PLACEMENT_3D ( 'NONE', #3554, #3765, #10358 ) ;
#14140 = CARTESIAN_POINT ( 'NONE',  ( 197.5000000000000000, -90.00000000000007105, 50.00000000000001421 ) ) ;
#14141 = SURFACE_SIDE_STYLE ('',( #5238 ) ) ;
#14142 = CARTESIAN_POINT ( 'NONE',  ( 134.9999999999999432, -56.99999999999997158, -169.9999999999999716 ) ) ;
#14143 = ITEM_DEFINED_TRANSFORMATION ( 'NONE', 'NONE', #4681,  #14039 ) ;
#14144 = CARTESIAN_POINT ( 'NONE',  ( -4.211405944401398038, -2.460460786169389902, -3.751298493805494072 ) ) ;
#14145 = VECTOR ( 'NONE', #7216, 1000.000000000000000 ) ;
#14146 = EDGE_LOOP ( 'NONE', ( #4373, #585, #6405, #11321 ) ) ;
#14147 = ORIENTED_EDGE ( 'NONE', *, *, #6843, .F. ) ;
#14148 = PLANE ( 'NONE',  #3135 ) ;
#14149 = ORIENTED_EDGE ( 'NONE', *, *, #7068, .T. ) ;
#14150 =( GEOMETRIC_REPRESENTATION_CONTEXT ( 3 ) GLOBAL_UNCERTAINTY_ASSIGNED_CONTEXT ( ( #4021 ) ) GLOBAL_UNIT_ASSIGNED_CONTEXT ( ( #13661, #5123, #9541 ) ) REPRESENTATION_CONTEXT ( 'NONE', 'WORKASPACE' ) );
#14151 = CARTESIAN_POINT ( 'NONE',  ( 319.9999999999999432, -225.0010000000000048, 19.99999999999998934 ) ) ;
#14152 = EDGE_LOOP ( 'NONE', ( #10872, #4153, #12805, #3059 ) ) ;
#14153 = EDGE_LOOP ( 'NONE', ( #12551, #9627, #13096, #9429 ) ) ;
#14154 = CARTESIAN_POINT ( 'NONE',  ( 140.0000000000000000, -75.00000000000008527, 186.2999999999999829 ) ) ;
#14155 = ORIENTED_EDGE ( 'NONE', *, *, #1843, .F. ) ;
#14156 = DIRECTION ( 'NONE',  ( 0.4461977533474923430, -0.8949343913984144638, 0.000000000000000000 ) ) ;
#14157 = LINE ( 'NONE', #11780, #12468 ) ;
#14158 = AXIS2_PLACEMENT_3D ( 'NONE', #5415, #9024, #8820 ) ;
#14159 = CARTESIAN_POINT ( 'NONE',  ( 200.8500000000000227, -85.00000000000007105, 55.00000000000001421 ) ) ;
#14160 = EDGE_CURVE ( 'NONE', #9074, #3667, #2968, .T. ) ;
#14161 = CARTESIAN_POINT ( 'NONE',  ( -20.63749999999999929, 0.000000000000000000, -9.999999999999996447 ) ) ;
#14162 = ORIENTED_EDGE ( 'NONE', *, *, #12977, .F. ) ;
#14163 = EDGE_CURVE ( 'NONE', #7984, #4156, #3653, .T. ) ;
#14164 = VERTEX_POINT ( 'NONE', #6087 ) ;
#14165 = VECTOR ( 'NONE', #4290, 1000.000000000000000 ) ;
#14166 = CIRCLE ( 'NONE', #2799, 10.20000000000000107 ) ;
#14167 = DIRECTION ( 'NONE',  ( 0.000000000000000000, 0.000000000000000000, 1.000000000000000000 ) ) ;
#14168 = EDGE_LOOP ( 'NONE', ( #1863, #10693, #4227 ) ) ;
#14169 = DIRECTION ( 'NONE',  ( -1.000000000000000000, 0.000000000000000000, 0.000000000000000000 ) ) ;
#14170 = CIRCLE ( 'NONE', #10241, 4.749999999999999112 ) ;
#14171 = DIRECTION ( 'NONE',  ( -1.000000000000000000, -0.000000000000000000, -0.000000000000000000 ) ) ;
#14172 = DIRECTION ( 'NONE',  ( -0.000000000000000000, -0.000000000000000000, -1.000000000000000000 ) ) ;
#14173 = ORIENTED_EDGE ( 'NONE', *, *, #6453, .T. ) ;
#14174 = CIRCLE ( 'NONE', #10727, 2.500000000000000444 ) ;
#14175 = CARTESIAN_POINT ( 'NONE',  ( 2.500000000000000000, 1.178949249685213863, -2.042000000000001148 ) ) ;
#14176 = AXIS2_PLACEMENT_3D ( 'NONE', #6904, #2346, #12021 ) ;
#14177 = DIRECTION ( 'NONE',  ( -0.000000000000000000, -0.000000000000000000, 1.000000000000000000 ) ) ;
#14178 = APPLICATION_PROTOCOL_DEFINITION ( 'draft international standard', 'automotive_design', 1998, #13774 ) ;
#14179 = CARTESIAN_POINT ( 'NONE',  ( 5.000000000000002665, 0.000000000000000000, -2.700000000000001066 ) ) ;
#14180 = EDGE_CURVE ( 'NONE', #8184, #4062, #6887, .T. ) ;
#14181 = ORIENTED_EDGE ( 'NONE', *, *, #5068, .T. ) ;
#14182 = EDGE_CURVE ( 'NONE', #67, #4723, #11767, .T. ) ;
#14183 =( REPRESENTATION_RELATIONSHIP ('NONE','NONE', #11251, #5332 ) REPRESENTATION_RELATIONSHIP_WITH_TRANSFORMATION ( #8784 )SHAPE_REPRESENTATION_RELATIONSHIP( ) );
#14184 = ORIENTED_EDGE ( 'NONE', *, *, #8818, .T. ) ;
#14185 = FACE_BOUND ( 'NONE', #10687, .T. ) ;
#14187 = AXIS2_PLACEMENT_3D ( 'NONE', #11766, #10752, #7182 ) ;
#14186 = VECTOR ( 'NONE', #13019, 1000.000000000000000 ) ;
#14188 = DIRECTION ( 'NONE',  ( 0.000000000000000000, 0.000000000000000000, -1.000000000000000000 ) ) ;
#14189 = DIRECTION ( 'NONE',  ( -1.000000000000000000, 0.000000000000000000, 0.000000000000000000 ) ) ;
#14190 = PRESENTATION_LAYER_ASSIGNMENT (  '', '', ( #4908 ) ) ;
#14191 = ORIENTED_EDGE ( 'NONE', *, *, #5693, .T. ) ;
#14192 = CARTESIAN_POINT ( 'NONE',  ( 2.500000000000000000, -1.178949249685213863, 2.042000000000002924 ) ) ;
#14193 = EDGE_CURVE ( 'NONE', #2276, #3217, #10332, .T. ) ;
#14194 = CARTESIAN_POINT ( 'NONE',  ( 2.500000000000000000, 2.357898499370433054, -1.951563910473907981E-15 ) ) ;
#14195 = PLANE ( 'NONE',  #9253 ) ;
#14196 = DIRECTION ( 'NONE',  ( 0.000000000000000000, 0.000000000000000000, 1.000000000000000000 ) ) ;
#14197 = CIRCLE ( 'NONE', #1213, 0.2000000000000022593 ) ;
#14198 = EDGE_CURVE ( 'NONE', #11965, #7334, #2268, .T. ) ;
#14199 = ORIENTED_EDGE ( 'NONE', *, *, #8161, .F. ) ;
#14200 = LINE ( 'NONE', #12105, #10558 ) ;
#14201 = ORIENTED_EDGE ( 'NONE', *, *, #4395, .F. ) ;
#14202 = CARTESIAN_POINT ( 'NONE',  ( 2.500000000000000000, 2.357898499370431722, -2.818925648462311528E-15 ) ) ;
#14203 = DIRECTION ( 'NONE',  ( 0.000000000000000000, -1.000000000000000000, 0.000000000000000000 ) ) ;
#14204 = ORIENTED_EDGE ( 'NONE', *, *, #10960, .T. ) ;
#14205 = EDGE_LOOP ( 'NONE', ( #7720, #4124 ) ) ;
#14206 = DIRECTION ( 'NONE',  ( -1.000000000000000000, -0.000000000000000000, -0.000000000000000000 ) ) ;
#14207 = EDGE_CURVE ( 'NONE', #9120, #3114, #1086, .T. ) ;
#14208 =( BOUNDED_SURFACE ( )  B_SPLINE_SURFACE ( 3, 2, ( 
 ( #3552, #2453, #6876 ),
 ( #4928, #11446, #11312 ),
 ( #249, #5863, #10355 ),
 ( #10432, #3615, #3481 ),
 ( #8025, #6948, #11379 ),
 ( #1429, #10285, #9198 ) ),
 .UNSPECIFIED., .F., .F., .F. ) 
 B_SPLINE_SURFACE_WITH_KNOTS ( ( 4, 2, 4 ),
 ( 3, 3 ),
 ( 0.02032853247518126225, 0.02278863295364821212, 0.02524873343211516200 ),
 ( 0.000000000000000000, 1.000000000000000000 ),
 .UNSPECIFIED. ) 
 GEOMETRIC_REPRESENTATION_ITEM ( )  RATIONAL_B_SPLINE_SURFACE ( (
 ( 1.000000000000000000, 0.8047781615896835161, 1.000000000000000000),
 ( 1.000000000000000000, 0.8123767586291043008, 1.000000000000000000),
 ( 1.000000000000000000, 0.8190662415562011134, 1.000000000000000000),
 ( 1.000000000000000000, 0.8192361015671398849, 1.000000000000000000),
 ( 1.000000000000000000, 0.8126135807102121689, 1.000000000000000000),
 ( 1.000000000000000000, 0.8047712338318585568, 1.000000000000000000) ) ) 
 REPRESENTATION_ITEM ( '' )  SURFACE ( )  );
#14209 = DIRECTION ( 'NONE',  ( -0.000000000000000000, -1.000000000000000000, -0.000000000000000000 ) ) ;
#14210 = ORIENTED_EDGE ( 'NONE', *, *, #5198, .F. ) ;
#14211 = DIRECTION ( 'NONE',  ( 0.000000000000000000, 0.000000000000000000, 1.000000000000000000 ) ) ;
#14212 = EDGE_CURVE ( 'NONE', #5643, #7514, #13332, .T. ) ;
#14213 = LINE ( 'NONE', #3279, #8666 ) ;
#14214 = DIRECTION ( 'NONE',  ( 0.000000000000000000, 0.000000000000000000, 1.000000000000000000 ) ) ;
#14215 = FILL_AREA_STYLE_COLOUR ( '', #9997 ) ;
#14216 = DIRECTION ( 'NONE',  ( 0.000000000000000000, 0.000000000000000000, 1.000000000000000000 ) ) ;
#14217 = EDGE_CURVE ( 'NONE', #2121, #3167, #10013, .T. ) ;
#14218 = DIRECTION ( 'NONE',  ( -1.000000000000000000, -0.000000000000000000, -0.000000000000000000 ) ) ;
#14219 = VERTEX_POINT ( 'NONE', #13270 ) ;
#14220 = ORIENTED_EDGE ( 'NONE', *, *, #6335, .T. ) ;
#14221 = CARTESIAN_POINT ( 'NONE',  ( 0.000000000000000000, 0.000000000000000000, 200.0000000000000000 ) ) ;
#14222 = EDGE_LOOP ( 'NONE', ( #14000, #10208, #10885, #5678 ) ) ;
#14223 = LINE ( 'NONE', #1153, #492 ) ;
#14224 = ORIENTED_EDGE ( 'NONE', *, *, #12757, .T. ) ;
#14225 = EDGE_LOOP ( 'NONE', ( #3287, #10506, #239, #8119 ) ) ;
#14226 = CARTESIAN_POINT ( 'NONE',  ( 0.000000000000000000, 0.000000000000000000, -186.0000000000000000 ) ) ;
#14227 = ORIENTED_EDGE ( 'NONE', *, *, #8942, .T. ) ;
#14228 = DIRECTION ( 'NONE',  ( -0.000000000000000000, -0.000000000000000000, 1.000000000000000000 ) ) ;
#14229 = CARTESIAN_POINT ( 'NONE',  ( 4.101954839143203912, 2.368264730583012234, -3.681130640444374436 ) ) ;
#14230 = DIRECTION ( 'NONE',  ( -1.000000000000000000, -0.000000000000000000, -0.000000000000000000 ) ) ;
#14231 = DIRECTION ( 'NONE',  ( 0.000000000000000000, 0.000000000000000000, -1.000000000000000000 ) ) ;
#14232 = DIRECTION ( 'NONE',  ( -0.000000000000000000, -0.000000000000000000, 1.000000000000000000 ) ) ;
#14233 = CARTESIAN_POINT ( 'NONE',  ( 145.0000000000000000, 55.00000000000000711, 0.000000000000000000 ) ) ;
#14234 = PRODUCT_DEFINITION_SHAPE ( 'NONE', 'NONE',  #14377 ) ;
#14235 = VERTEX_POINT ( 'NONE', #914 ) ;
#14236 = ORIENTED_EDGE ( 'NONE', *, *, #13846, .T. ) ;
#14237 = EDGE_CURVE ( 'NONE', #2397, #4974, #12254, .T. ) ;
#14238 = DIRECTION ( 'NONE',  ( -0.000000000000000000, 1.000000000000000000, -0.000000000000000000 ) ) ;
#14239 = ORIENTED_EDGE ( 'NONE', *, *, #1007, .F. ) ;
#14240 = CARTESIAN_POINT ( 'NONE',  ( 1.424271237134740131, 0.000000000000000000, 0.000000000000000000 ) ) ;
#14241 = CARTESIAN_POINT ( 'NONE',  ( 4.211140560182196957, -2.431303136016555122, -3.745885042887436622 ) ) ;
#14242 = CIRCLE ( 'NONE', #9853, 8.000000000000000000 ) ;
#14243 = CIRCLE ( 'NONE', #1027, 2.649999999999985700 ) ;
#14244 = EDGE_LOOP ( 'NONE', ( #6301, #4711, #5267 ) ) ;
#14245 = DIRECTION ( 'NONE',  ( 1.007709689656716938E-16, 1.153406566473941260E-16, -1.000000000000000000 ) ) ;
#14246 = CARTESIAN_POINT ( 'NONE',  ( 238.9999999999999432, -85.00000000000007105, 180.0000000000000000 ) ) ;
#14247 = DIRECTION ( 'NONE',  ( 1.000000000000000000, 0.000000000000000000, -6.123233995736766036E-17 ) ) ;
#14248 = PLANE ( 'NONE',  #10075 ) ;
#14249 = ORIENTED_EDGE ( 'NONE', *, *, #6715, .T. ) ;
#14250 = AXIS2_PLACEMENT_3D ( 'NONE', #9963, #3369, #5667 ) ;
#14251 = EDGE_CURVE ( 'NONE', #722, #1400, #7749, .T. ) ;
#14252 = AXIS2_PLACEMENT_3D ( 'NONE', #1346, #11372, #11306 ) ;
#14253 = VERTEX_POINT ( 'NONE', #12115 ) ;
#14254 = CARTESIAN_POINT ( 'NONE',  ( 0.000000000000000000, 0.000000000000000000, 0.000000000000000000 ) ) ;
#14255 = CARTESIAN_POINT ( 'NONE',  ( -304.9999999999999432, -75.00000000000008527, 0.000000000000000000 ) ) ;
#14256 = VERTEX_POINT ( 'NONE', #2028 ) ;
#14258 = ADVANCED_FACE ( 'NONE', ( #3352 ), #8703, .F. ) ;
#14257 = CARTESIAN_POINT ( 'NONE',  ( 1.654252653721905331, 3.663718938583014229, -0.01223254789873410957 ) ) ;
#14259 = VECTOR ( 'NONE', #11168, 1000.000000000000000 ) ;
#14260 = ADVANCED_FACE ( 'NONE', ( #42 ), #4501, .T. ) ;
#14261 = CARTESIAN_POINT ( 'NONE',  ( 3.333333333333335702, -2.694301256218268215, -3.300726591567084256 ) ) ;
#14262 = AXIS2_PLACEMENT_3D ( 'NONE', #312, #1354, #7086 ) ;
#14263 = DIRECTION ( 'NONE',  ( 1.000000000000000000, 0.000000000000000000, 0.000000000000000000 ) ) ;
#14264 = CARTESIAN_POINT ( 'NONE',  ( 352.0000000000000000, 0.000000000000000000, -188.0000000000000000 ) ) ;
#14265 = CIRCLE ( 'NONE', #13346, 2.649999999999985700 ) ;
#14266 = EDGE_LOOP ( 'NONE', ( #9328, #5265, #1117, #13569 ) ) ;
#14267 = CARTESIAN_POINT ( 'NONE',  ( -2.000000000000001776, 1.564486285910744042E-15, 12.77500000000000213 ) ) ;
#14268 = VERTEX_POINT ( 'NONE', #3416 ) ;
#14269 = CARTESIAN_POINT ( 'NONE',  ( 4.999999999999999112, -8.660254037844389075, -210.0000000000000000 ) ) ;
#14270 = CARTESIAN_POINT ( 'NONE',  ( 1.424271237134740131, 4.556291390728479662, 0.000000000000000000 ) ) ;
#14271 = CIRCLE ( 'NONE', #2702, 2.500000000000002220 ) ;
#14272 = EDGE_LOOP ( 'NONE', ( #11042, #1081, #13007, #8337, #589 ) ) ;
#14273 = ORIENTED_EDGE ( 'NONE', *, *, #8434, .T. ) ;
#14275 = ADVANCED_FACE ( 'NONE', ( #10965 ), #2358, .F. ) ;
#14274 = DIRECTION ( 'NONE',  ( 0.000000000000000000, 0.000000000000000000, -1.000000000000000000 ) ) ;
#14276 = EDGE_CURVE ( 'NONE', #794, #568, #11237, .T. ) ;
#14277 = CARTESIAN_POINT ( 'NONE',  ( -3.472371940586054251, -2.614027278893156669, -3.320322319202162031 ) ) ;
#14278 = VECTOR ( 'NONE', #7164, 1000.000000000000000 ) ;
#14279 = AXIS2_PLACEMENT_3D ( 'NONE', #9996, #10200, #4702 ) ;
#14280 = CARTESIAN_POINT ( 'NONE',  ( 4.211140560182196957, 2.431303136016536470, -3.745885042887433514 ) ) ;
#14281 = CIRCLE ( 'NONE', #12446, 10.72500000000000142 ) ;
#14282 = LINE ( 'NONE', #13128, #14165 ) ;
#14283 = DIRECTION ( 'NONE',  ( 0.000000000000000000, 0.000000000000000000, 1.000000000000000000 ) ) ;
#14284 = PLANE ( 'NONE',  #1115 ) ;
#14285 = CONTEXT_DEPENDENT_SHAPE_REPRESENTATION ( #1171, #13515 ) ;
#14286 = AXIS2_PLACEMENT_3D ( 'NONE', #10982, #7554, #4379 ) ;
#14287 = VECTOR ( 'NONE', #9823, 1000.000000000000000 ) ;
#14288 = ORIENTED_EDGE ( 'NONE', *, *, #6270, .T. ) ;
#14289 = EDGE_LOOP ( 'NONE', ( #3807, #12125, #5031, #7421, #6058 ) ) ;
#14290 = EDGE_CURVE ( 'NONE', #5230, #2239, #341, .T. ) ;
#14291 = EDGE_CURVE ( 'NONE', #8299, #8193, #7025, .T. ) ;
#14292 = FACE_OUTER_BOUND ( 'NONE', #5944, .T. ) ;
#14293 = ORIENTED_EDGE ( 'NONE', *, *, #13935, .F. ) ;
#14294 = EDGE_CURVE ( 'NONE', #6925, #7098, #10365, .T. ) ;
#14295 = CARTESIAN_POINT ( 'NONE',  ( -4.154094228333542915, 2.398367420968061658, -3.721909803043254694 ) ) ;
#14296 = ORIENTED_EDGE ( 'NONE', *, *, #7726, .F. ) ;
#14297 = AXIS2_PLACEMENT_3D ( 'NONE', #11833, #6318, #3064 ) ;
#14298 = EDGE_LOOP ( 'NONE', ( #12322, #2132, #726, #7553 ) ) ;
#14299 = DIRECTION ( 'NONE',  ( 0.000000000000000000, 0.000000000000000000, -1.000000000000000000 ) ) ;
#14300 = EDGE_LOOP ( 'NONE', ( #4320, #10832, #14220, #11988 ) ) ;
#14301 = CARTESIAN_POINT ( 'NONE',  ( 0.9586399445693771781, -0.8293189044373066032, -0.5150000000000000133 ) ) ;
#14302 = AXIS2_PLACEMENT_3D ( 'NONE', #700, #12691, #4063 ) ;
#14303 = VECTOR ( 'NONE', #11972, 1000.000000000000000 ) ;
#14304 = FACE_OUTER_BOUND ( 'NONE', #752, .T. ) ;
#14305 = LINE ( 'NONE', #4307, #7796 ) ;
#14306 = ORIENTED_EDGE ( 'NONE', *, *, #10530, .T. ) ;
#14307 = NEXT_ASSEMBLY_USAGE_OCCURRENCE ( 'NAUO1', ' ', ' ', #75, #5767, $ ) ;
#14308 = NEXT_ASSEMBLY_USAGE_OCCURRENCE ( 'NAUO2', ' ', ' ', #75, #5595, $ ) ;
#14309 = NEXT_ASSEMBLY_USAGE_OCCURRENCE ( 'NAUO3', ' ', ' ', #75, #13657, $ ) ;
#14310 = NEXT_ASSEMBLY_USAGE_OCCURRENCE ( 'NAUO4', ' ', ' ', #75, #2142, $ ) ;
#14311 = NEXT_ASSEMBLY_USAGE_OCCURRENCE ( 'NAUO5', ' ', ' ', #75, #6314, $ ) ;
#14312 = NEXT_ASSEMBLY_USAGE_OCCURRENCE ( 'NAUO6', ' ', ' ', #75, #6314, $ ) ;
#14313 = NEXT_ASSEMBLY_USAGE_OCCURRENCE ( 'NAUO7', ' ', ' ', #75, #13043, $ ) ;
#14314 = NEXT_ASSEMBLY_USAGE_OCCURRENCE ( 'NAUO8', ' ', ' ', #75, #13043, $ ) ;
#14315 = NEXT_ASSEMBLY_USAGE_OCCURRENCE ( 'NAUO9', ' ', ' ', #75, #13043, $ ) ;
#14316 = NEXT_ASSEMBLY_USAGE_OCCURRENCE ( 'NAUO10', ' ', ' ', #75, #13043, $ ) ;
#14317 = NEXT_ASSEMBLY_USAGE_OCCURRENCE ( 'NAUO11', ' ', ' ', #75, #13043, $ ) ;
#14318 = NEXT_ASSEMBLY_USAGE_OCCURRENCE ( 'NAUO12', ' ', ' ', #75, #10925, $ ) ;
#14319 = NEXT_ASSEMBLY_USAGE_OCCURRENCE ( 'NAUO13', ' ', ' ', #75, #10925, $ ) ;
#14320 = NEXT_ASSEMBLY_USAGE_OCCURRENCE ( 'NAUO14', ' ', ' ', #75, #10925, $ ) ;
#14321 = NEXT_ASSEMBLY_USAGE_OCCURRENCE ( 'NAUO15', ' ', ' ', #75, #10925, $ ) ;
#14322 = NEXT_ASSEMBLY_USAGE_OCCURRENCE ( 'NAUO16', ' ', ' ', #75, #10925, $ ) ;
#14323 = NEXT_ASSEMBLY_USAGE_OCCURRENCE ( 'NAUO17', ' ', ' ', #75, #13657, $ ) ;
#14324 = NEXT_ASSEMBLY_USAGE_OCCURRENCE ( 'NAUO18', ' ', ' ', #75, #6314, $ ) ;
#14325 = NEXT_ASSEMBLY_USAGE_OCCURRENCE ( 'NAUO19', ' ', ' ', #75, #6314, $ ) ;
#14326 = NEXT_ASSEMBLY_USAGE_OCCURRENCE ( 'NAUO20', ' ', ' ', #75, #6314, $ ) ;
#14327 = NEXT_ASSEMBLY_USAGE_OCCURRENCE ( 'NAUO21', ' ', ' ', #75, #6314, $ ) ;
#14328 = NEXT_ASSEMBLY_USAGE_OCCURRENCE ( 'NAUO22', ' ', ' ', #75, #6314, $ ) ;
#14329 = NEXT_ASSEMBLY_USAGE_OCCURRENCE ( 'NAUO23', ' ', ' ', #75, #5767, $ ) ;
#14330 = NEXT_ASSEMBLY_USAGE_OCCURRENCE ( 'NAUO24', ' ', ' ', #75, #5767, $ ) ;
#14331 = NEXT_ASSEMBLY_USAGE_OCCURRENCE ( 'NAUO25', ' ', ' ', #75, #5767, $ ) ;
#14332 = NEXT_ASSEMBLY_USAGE_OCCURRENCE ( 'NAUO26', ' ', ' ', #75, #5767, $ ) ;
#14333 = NEXT_ASSEMBLY_USAGE_OCCURRENCE ( 'NAUO27', ' ', ' ', #75, #5767, $ ) ;
#14334 = NEXT_ASSEMBLY_USAGE_OCCURRENCE ( 'NAUO28', ' ', ' ', #75, #6314, $ ) ;
#14335 = NEXT_ASSEMBLY_USAGE_OCCURRENCE ( 'NAUO29', ' ', ' ', #75, #6314, $ ) ;
#14336 = NEXT_ASSEMBLY_USAGE_OCCURRENCE ( 'NAUO30', ' ', ' ', #75, #6314, $ ) ;
#14337 = NEXT_ASSEMBLY_USAGE_OCCURRENCE ( 'NAUO31', ' ', ' ', #75, #6314, $ ) ;
#14338 = NEXT_ASSEMBLY_USAGE_OCCURRENCE ( 'NAUO32', ' ', ' ', #75, #6314, $ ) ;
#14339 = NEXT_ASSEMBLY_USAGE_OCCURRENCE ( 'NAUO33', ' ', ' ', #75, #5595, $ ) ;
#14340 = NEXT_ASSEMBLY_USAGE_OCCURRENCE ( 'NAUO34', ' ', ' ', #75, #5595, $ ) ;
#14341 = NEXT_ASSEMBLY_USAGE_OCCURRENCE ( 'NAUO35', ' ', ' ', #75, #5595, $ ) ;
#14342 = NEXT_ASSEMBLY_USAGE_OCCURRENCE ( 'NAUO36', ' ', ' ', #75, #5595, $ ) ;
#14343 = NEXT_ASSEMBLY_USAGE_OCCURRENCE ( 'NAUO37', ' ', ' ', #75, #5595, $ ) ;
#14344 = NEXT_ASSEMBLY_USAGE_OCCURRENCE ( 'NAUO38', ' ', ' ', #75, #10925, $ ) ;
#14345 = NEXT_ASSEMBLY_USAGE_OCCURRENCE ( 'NAUO39', ' ', ' ', #75, #10925, $ ) ;
#14346 = NEXT_ASSEMBLY_USAGE_OCCURRENCE ( 'NAUO40', ' ', ' ', #75, #13043, $ ) ;
#14347 = NEXT_ASSEMBLY_USAGE_OCCURRENCE ( 'NAUO41', ' ', ' ', #75, #10925, $ ) ;
#14348 = NEXT_ASSEMBLY_USAGE_OCCURRENCE ( 'NAUO42', ' ', ' ', #75, #13043, $ ) ;
#14349 = NEXT_ASSEMBLY_USAGE_OCCURRENCE ( 'NAUO43', ' ', ' ', #75, #13043, $ ) ;
#14350 = NEXT_ASSEMBLY_USAGE_OCCURRENCE ( 'NAUO44', ' ', ' ', #75, #13043, $ ) ;
#14351 = NEXT_ASSEMBLY_USAGE_OCCURRENCE ( 'NAUO45', ' ', ' ', #75, #13043, $ ) ;
#14352 = NEXT_ASSEMBLY_USAGE_OCCURRENCE ( 'NAUO46', ' ', ' ', #75, #10925, $ ) ;
#14353 = NEXT_ASSEMBLY_USAGE_OCCURRENCE ( 'NAUO47', ' ', ' ', #75, #10925, $ ) ;
#14354 = NEXT_ASSEMBLY_USAGE_OCCURRENCE ( 'NAUO48', ' ', ' ', #75, #12238, $ ) ;
#14355 = NEXT_ASSEMBLY_USAGE_OCCURRENCE ( 'NAUO49', ' ', ' ', #75, #6833, $ ) ;
#14356 = NEXT_ASSEMBLY_USAGE_OCCURRENCE ( 'NAUO50', ' ', ' ', #75, #12238, $ ) ;
#14357 = NEXT_ASSEMBLY_USAGE_OCCURRENCE ( 'NAUO51', ' ', ' ', #75, #5165, $ ) ;
#14358 = NEXT_ASSEMBLY_USAGE_OCCURRENCE ( 'NAUO52', ' ', ' ', #75, #5165, $ ) ;
#14359 = NEXT_ASSEMBLY_USAGE_OCCURRENCE ( 'NAUO53', ' ', ' ', #75, #5165, $ ) ;
#14360 = NEXT_ASSEMBLY_USAGE_OCCURRENCE ( 'NAUO54', ' ', ' ', #75, #5165, $ ) ;
#14361 = NEXT_ASSEMBLY_USAGE_OCCURRENCE ( 'NAUO55', ' ', ' ', #75, #3819, $ ) ;
#14362 = NEXT_ASSEMBLY_USAGE_OCCURRENCE ( 'NAUO56', ' ', ' ', #75, #6833, $ ) ;
#14363 = NEXT_ASSEMBLY_USAGE_OCCURRENCE ( 'NAUO57', ' ', ' ', #75, #1870, $ ) ;
#14364 = NEXT_ASSEMBLY_USAGE_OCCURRENCE ( 'NAUO58', ' ', ' ', #75, #10925, $ ) ;
#14365 = NEXT_ASSEMBLY_USAGE_OCCURRENCE ( 'NAUO59', ' ', ' ', #75, #8151, $ ) ;
#14366 = NEXT_ASSEMBLY_USAGE_OCCURRENCE ( 'NAUO60', ' ', ' ', #75, #8151, $ ) ;
#14367 = NEXT_ASSEMBLY_USAGE_OCCURRENCE ( 'NAUO61', ' ', ' ', #75, #8151, $ ) ;
#14368 = NEXT_ASSEMBLY_USAGE_OCCURRENCE ( 'NAUO62', ' ', ' ', #75, #8151, $ ) ;
#14369 = NEXT_ASSEMBLY_USAGE_OCCURRENCE ( 'NAUO63', ' ', ' ', #75, #1599, $ ) ;
#14370 = NEXT_ASSEMBLY_USAGE_OCCURRENCE ( 'NAUO64', ' ', ' ', #75, #1599, $ ) ;
#14371 = NEXT_ASSEMBLY_USAGE_OCCURRENCE ( 'NAUO65', ' ', ' ', #75, #13043, $ ) ;
#14372 = NEXT_ASSEMBLY_USAGE_OCCURRENCE ( 'NAUO66', ' ', ' ', #75, #13043, $ ) ;
#14373 = NEXT_ASSEMBLY_USAGE_OCCURRENCE ( 'NAUO67', ' ', ' ', #75, #8151, $ ) ;
#14374 = NEXT_ASSEMBLY_USAGE_OCCURRENCE ( 'NAUO68', ' ', ' ', #75, #8151, $ ) ;
#14375 = NEXT_ASSEMBLY_USAGE_OCCURRENCE ( 'NAUO69', ' ', ' ', #75, #8151, $ ) ;
#14376 = NEXT_ASSEMBLY_USAGE_OCCURRENCE ( 'NAUO70', ' ', ' ', #75, #8151, $ ) ;
#14377 = NEXT_ASSEMBLY_USAGE_OCCURRENCE ( 'NAUO71', ' ', ' ', #75, #8892, $ ) ;
#14378 = NEXT_ASSEMBLY_USAGE_OCCURRENCE ( 'NAUO72', ' ', ' ', #75, #8892, $ ) ;
#14379 = NEXT_ASSEMBLY_USAGE_OCCURRENCE ( 'NAUO73', ' ', ' ', #75, #8892, $ ) ;
#14380 = NEXT_ASSEMBLY_USAGE_OCCURRENCE ( 'NAUO74', ' ', ' ', #75, #8892, $ ) ;
#14381 = NEXT_ASSEMBLY_USAGE_OCCURRENCE ( 'NAUO75', ' ', ' ', #75, #13043, $ ) ;
#14382 = NEXT_ASSEMBLY_USAGE_OCCURRENCE ( 'NAUO76', ' ', ' ', #75, #13043, $ ) ;
#14383=COLOUR_RGB('Dark Blue',0.08,0.2,0.34);
#14384=FILL_AREA_STYLE_COLOUR('',#14383);
#14385=FILL_AREA_STYLE('',(#14384));
#14386=SURFACE_STYLE_FILL_AREA(#14385);
#14387=SURFACE_SIDE_STYLE('',(#14386));
#14388=SURFACE_STYLE_USAGE(.BOTH.,#14387);
#14389=PRESENTATION_STYLE_ASSIGNMENT((#14388));
#14390=COLOUR_RGB('Light Blue',0.38,0.62,0.78);
#14391=FILL_AREA_STYLE_COLOUR('',#14390);
#14392=FILL_AREA_STYLE('',(#14391));
#14393=SURFACE_STYLE_FILL_AREA(#14392);
#14394=SURFACE_SIDE_STYLE('',(#14393));
#14395=SURFACE_STYLE_USAGE(.BOTH.,#14394);
#14396=PRESENTATION_STYLE_ASSIGNMENT((#14395));
#14397=COLOUR_RGB('Sky Blue',0.24,0.69,0.87);
#14398=FILL_AREA_STYLE_COLOUR('',#14397);
#14399=FILL_AREA_STYLE('',(#14398));
#14400=SURFACE_STYLE_FILL_AREA(#14399);
#14401=SURFACE_SIDE_STYLE('',(#14400));
#14402=SURFACE_STYLE_USAGE(.BOTH.,#14401);
#14403=PRESENTATION_STYLE_ASSIGNMENT((#14402));
#14404=COLOUR_RGB('Grey',0.48,0.52,0.57);
#14405=FILL_AREA_STYLE_COLOUR('',#14404);
#14406=FILL_AREA_STYLE('',(#14405));
#14407=SURFACE_STYLE_FILL_AREA(#14406);
#14408=SURFACE_SIDE_STYLE('',(#14407));
#14409=SURFACE_STYLE_USAGE(.BOTH.,#14408);
#14410=PRESENTATION_STYLE_ASSIGNMENT((#14409));
#14411=COLOUR_RGB('Black',0.12,0.14,0.17);
#14412=FILL_AREA_STYLE_COLOUR('',#14411);
#14413=FILL_AREA_STYLE('',(#14412));
#14414=SURFACE_STYLE_FILL_AREA(#14413);
#14415=SURFACE_SIDE_STYLE('',(#14414));
#14416=SURFACE_STYLE_USAGE(.BOTH.,#14415);
#14417=PRESENTATION_STYLE_ASSIGNMENT((#14416));
#14418=COLOUR_RGB('Off White',0.89,0.88,0.83);
#14419=FILL_AREA_STYLE_COLOUR('',#14418);
#14420=FILL_AREA_STYLE('',(#14419));
#14421=SURFACE_STYLE_FILL_AREA(#14420);
#14422=SURFACE_SIDE_STYLE('',(#14421));
#14423=SURFACE_STYLE_USAGE(.BOTH.,#14422);
#14424=PRESENTATION_STYLE_ASSIGNMENT((#14423));
ENDSEC;
END-ISO-10303-21;
